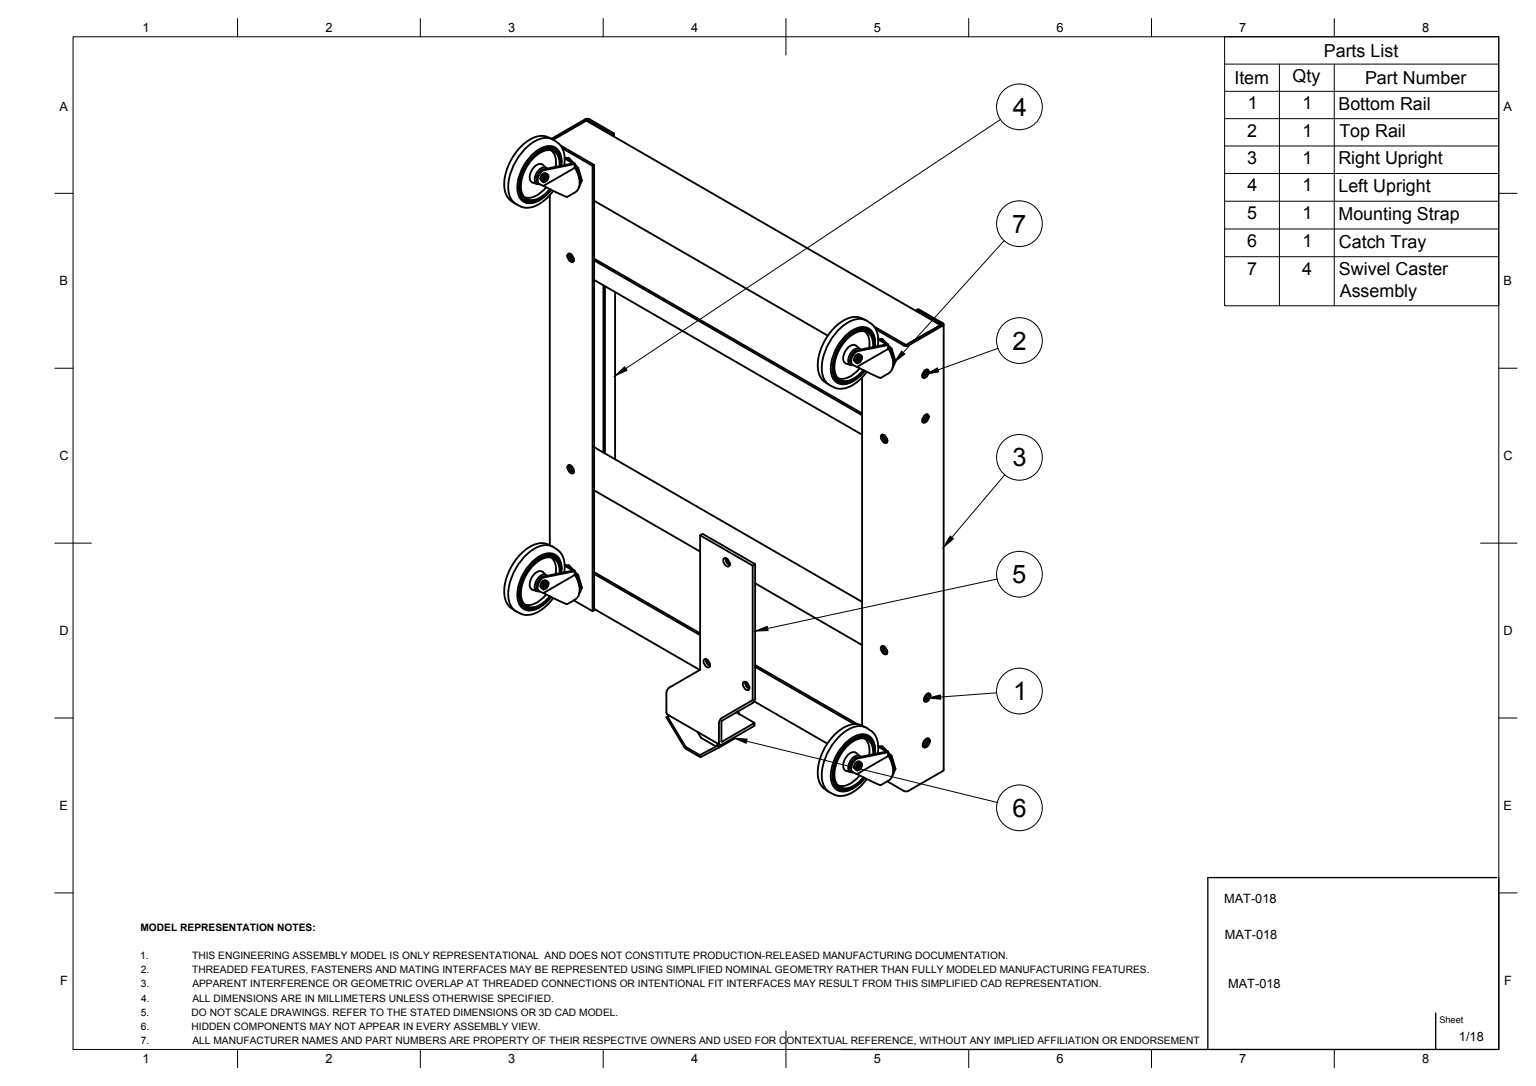
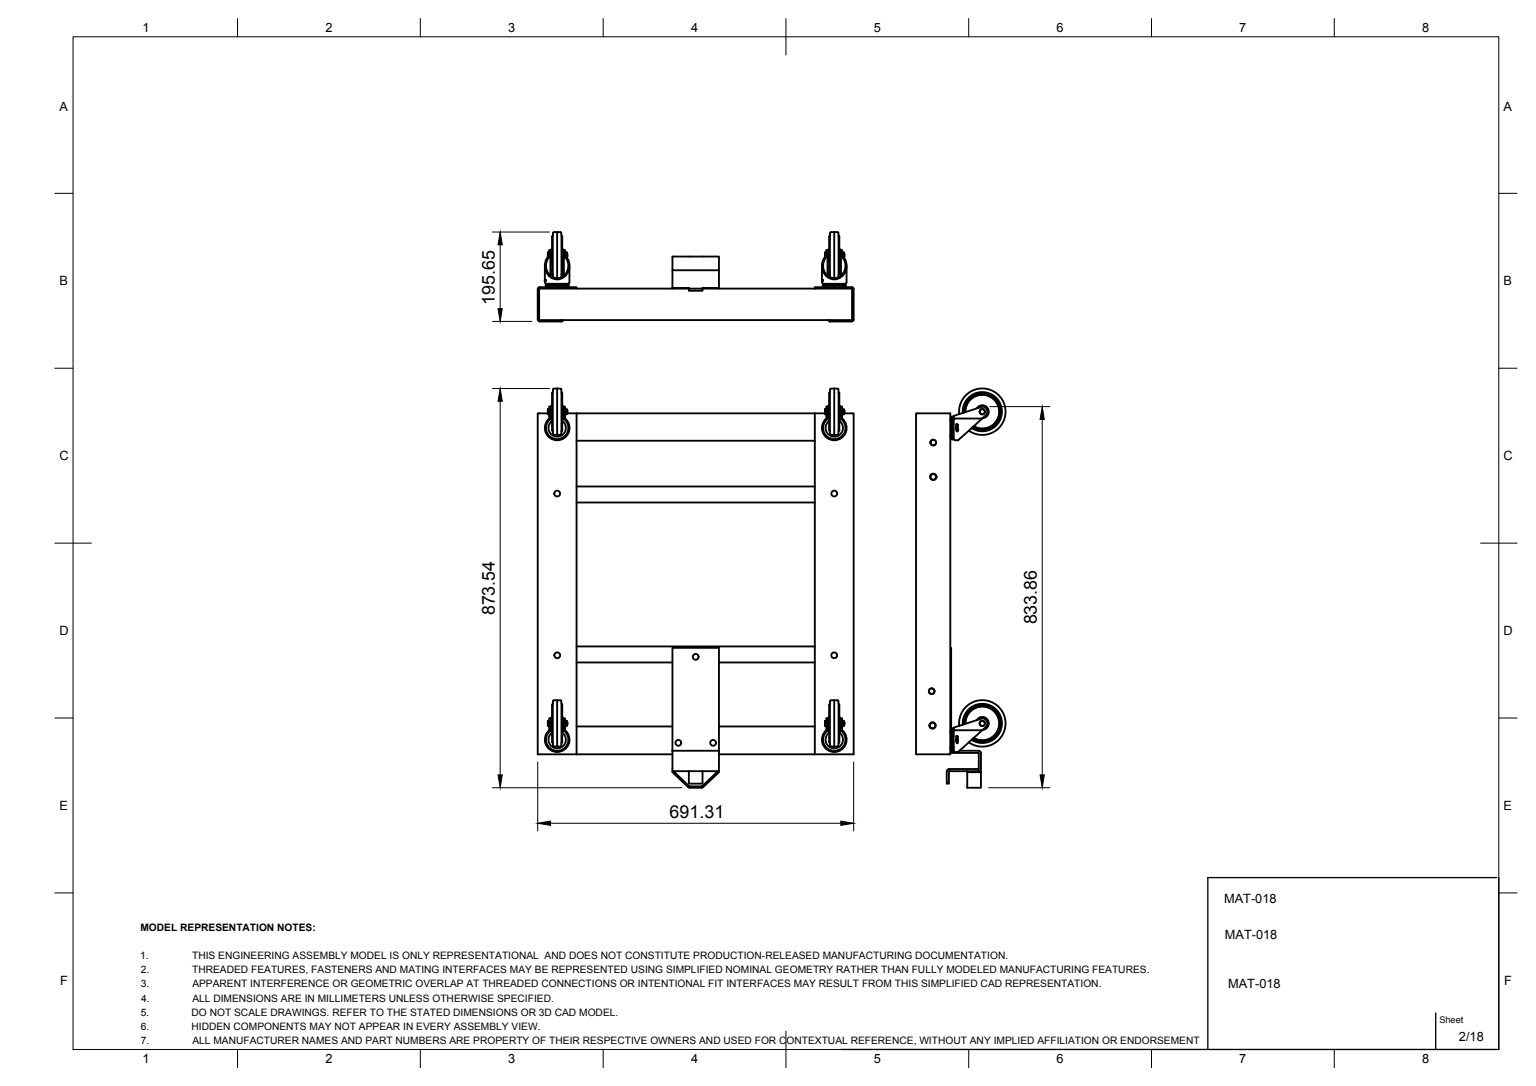
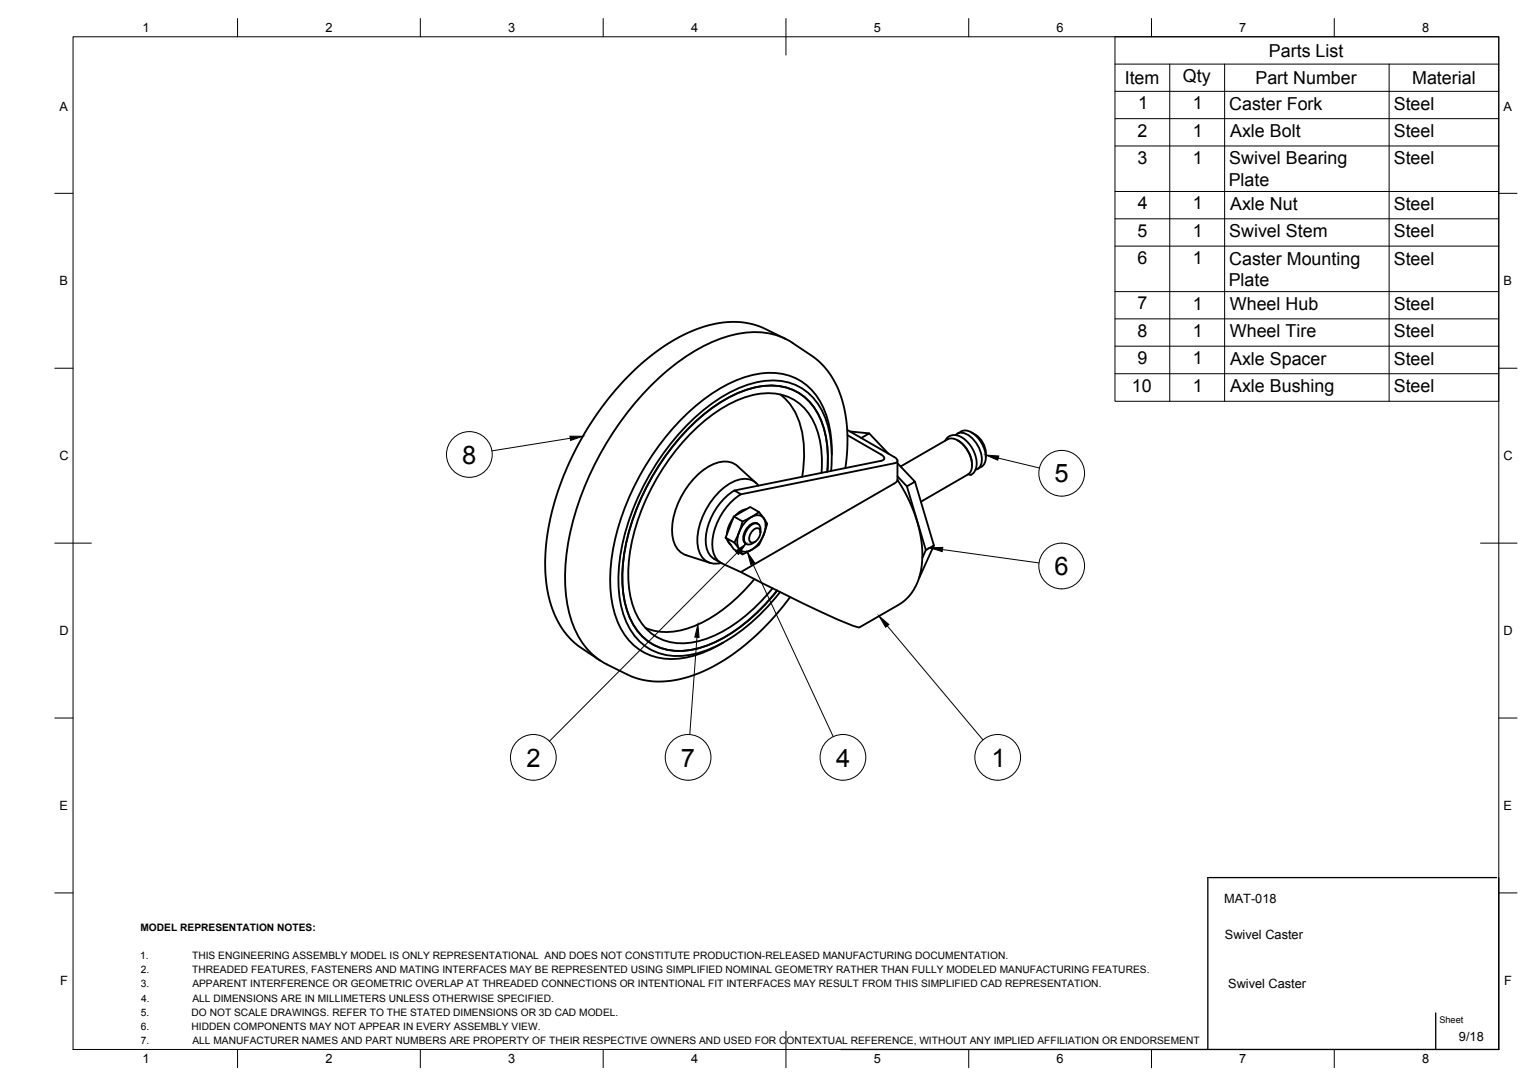
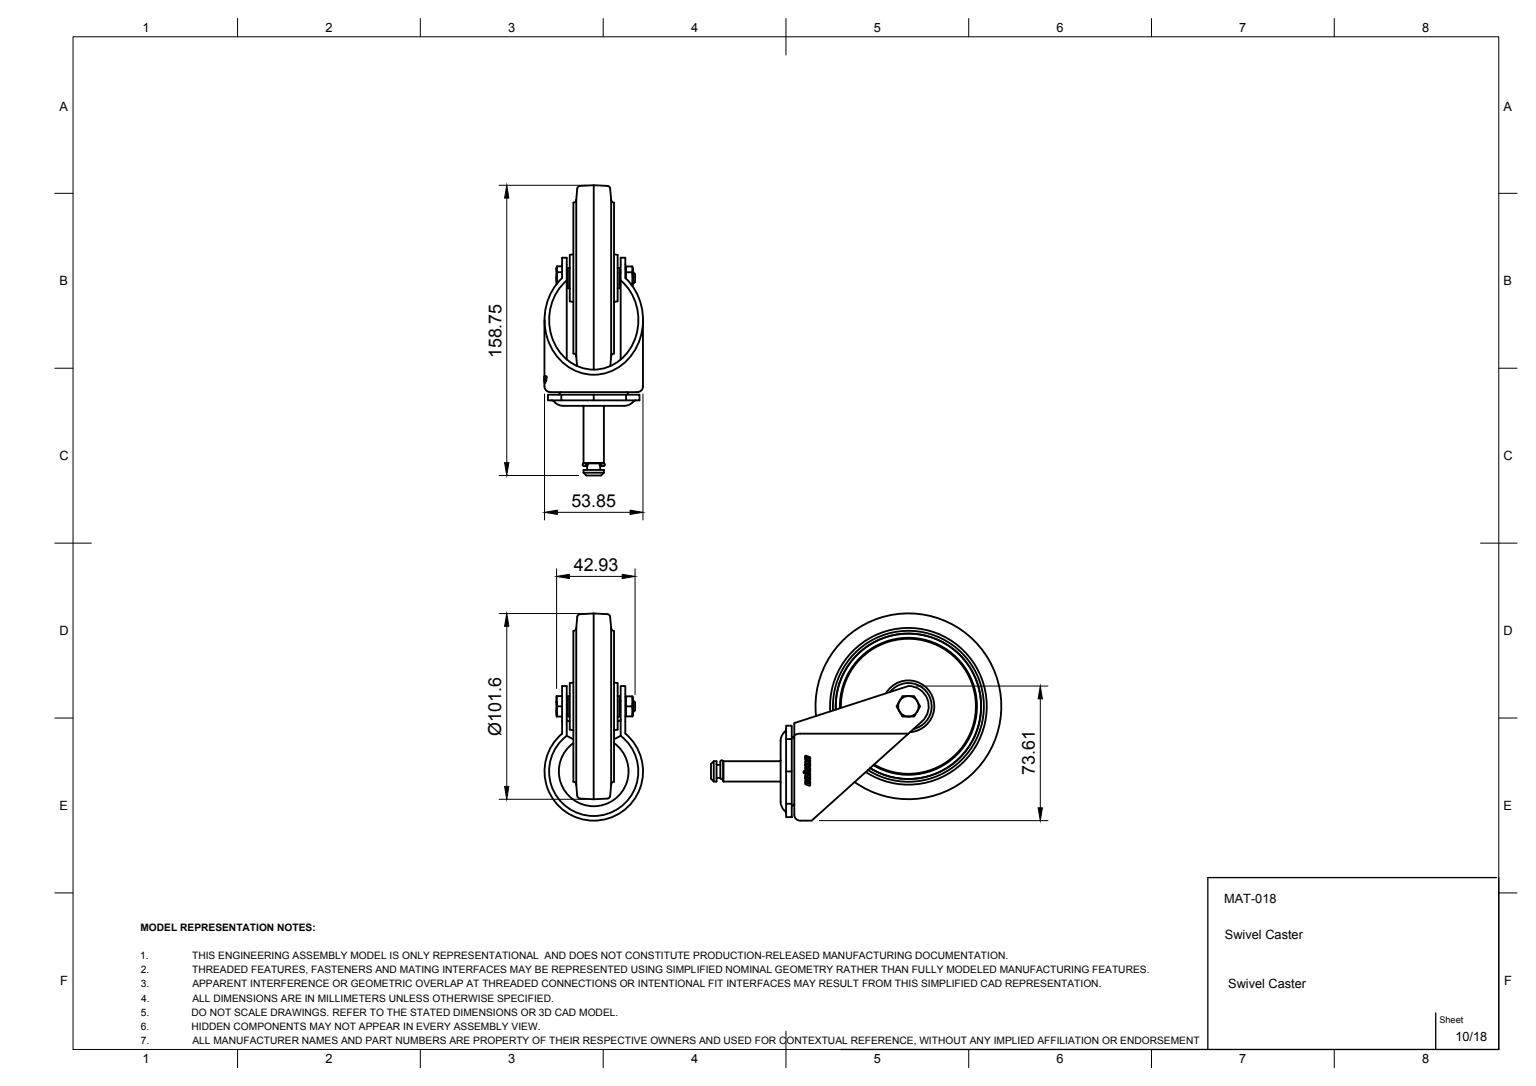
ISO-10303-21;
HEADER;
/* Generated by software containing ST-Developer
 * from STEP Tools, Inc. (www.steptools.com) 
 */

FILE_DESCRIPTION(
/* description */ ('STEP AP214'),
/* implementation_level */ '2;1');

FILE_NAME(
/* name */ 'MAT-018.step',
/* time_stamp */ '2026-11-14T06:16:09-08:00',
/* author */ (''),
/* organization */ (''),
/* preprocessor_version */ 'ST-DEVELOPER v20.2',
/* originating_system */ 'Autodesk Translation Framework v15.17.0.0',
/* authorisation */ '');

FILE_SCHEMA (('AUTOMOTIVE_DESIGN { 1 0 10303 214 3 1 1 }'));
ENDSEC;

DATA;
#10=MECHANICAL_DESIGN_GEOMETRIC_PRESENTATION_REPRESENTATION('',(#347,#348,
#349,#350,#351,#352,#353,#354,#355,#356,#357,#358,#359,#360,#361,#362),
#18006);
#11=ITEM_DEFINED_TRANSFORMATION($,$,#10244,#10840);
#12=ITEM_DEFINED_TRANSFORMATION($,$,#10508,#10841);
#13=ITEM_DEFINED_TRANSFORMATION($,$,#10546,#10842);
#14=ITEM_DEFINED_TRANSFORMATION($,$,#10592,#10843);
#15=ITEM_DEFINED_TRANSFORMATION($,$,#10635,#10844);
#16=ITEM_DEFINED_TRANSFORMATION($,$,#10683,#10845);
#17=ITEM_DEFINED_TRANSFORMATION($,$,#10733,#10846);
#18=ITEM_DEFINED_TRANSFORMATION($,$,#10772,#10847);
#19=ITEM_DEFINED_TRANSFORMATION($,$,#10817,#10848);
#20=ITEM_DEFINED_TRANSFORMATION($,$,#10826,#10849);
#21=ITEM_DEFINED_TRANSFORMATION($,$,#10243,#10850);
#22=ITEM_DEFINED_TRANSFORMATION($,$,#9750,#10851);
#23=ITEM_DEFINED_TRANSFORMATION($,$,#9886,#10852);
#24=ITEM_DEFINED_TRANSFORMATION($,$,#10013,#10853);
#25=ITEM_DEFINED_TRANSFORMATION($,$,#10080,#10854);
#26=ITEM_DEFINED_TRANSFORMATION($,$,#10147,#10855);
#27=ITEM_DEFINED_TRANSFORMATION($,$,#10211,#10856);
#28=ITEM_DEFINED_TRANSFORMATION($,$,#10242,#10857);
#29=ITEM_DEFINED_TRANSFORMATION($,$,#10242,#10858);
#30=ITEM_DEFINED_TRANSFORMATION($,$,#10242,#10859);
#31=ITEM_DEFINED_TRANSFORMATION($,$,#10242,#10860);
#32=(
REPRESENTATION_RELATIONSHIP($,$,#18079,#18078)
REPRESENTATION_RELATIONSHIP_WITH_TRANSFORMATION(#11)
SHAPE_REPRESENTATION_RELATIONSHIP()
);
#33=(
REPRESENTATION_RELATIONSHIP($,$,#18080,#18078)
REPRESENTATION_RELATIONSHIP_WITH_TRANSFORMATION(#12)
SHAPE_REPRESENTATION_RELATIONSHIP()
);
#34=(
REPRESENTATION_RELATIONSHIP($,$,#18081,#18078)
REPRESENTATION_RELATIONSHIP_WITH_TRANSFORMATION(#13)
SHAPE_REPRESENTATION_RELATIONSHIP()
);
#35=(
REPRESENTATION_RELATIONSHIP($,$,#18082,#18078)
REPRESENTATION_RELATIONSHIP_WITH_TRANSFORMATION(#14)
SHAPE_REPRESENTATION_RELATIONSHIP()
);
#36=(
REPRESENTATION_RELATIONSHIP($,$,#18083,#18078)
REPRESENTATION_RELATIONSHIP_WITH_TRANSFORMATION(#15)
SHAPE_REPRESENTATION_RELATIONSHIP()
);
#37=(
REPRESENTATION_RELATIONSHIP($,$,#18084,#18078)
REPRESENTATION_RELATIONSHIP_WITH_TRANSFORMATION(#16)
SHAPE_REPRESENTATION_RELATIONSHIP()
);
#38=(
REPRESENTATION_RELATIONSHIP($,$,#18085,#18078)
REPRESENTATION_RELATIONSHIP_WITH_TRANSFORMATION(#17)
SHAPE_REPRESENTATION_RELATIONSHIP()
);
#39=(
REPRESENTATION_RELATIONSHIP($,$,#18086,#18078)
REPRESENTATION_RELATIONSHIP_WITH_TRANSFORMATION(#18)
SHAPE_REPRESENTATION_RELATIONSHIP()
);
#40=(
REPRESENTATION_RELATIONSHIP($,$,#18087,#18078)
REPRESENTATION_RELATIONSHIP_WITH_TRANSFORMATION(#19)
SHAPE_REPRESENTATION_RELATIONSHIP()
);
#41=(
REPRESENTATION_RELATIONSHIP($,$,#18088,#18078)
REPRESENTATION_RELATIONSHIP_WITH_TRANSFORMATION(#20)
SHAPE_REPRESENTATION_RELATIONSHIP()
);
#42=(
REPRESENTATION_RELATIONSHIP($,$,#18078,#18077)
REPRESENTATION_RELATIONSHIP_WITH_TRANSFORMATION(#21)
SHAPE_REPRESENTATION_RELATIONSHIP()
);
#43=(
REPRESENTATION_RELATIONSHIP($,$,#18071,#18070)
REPRESENTATION_RELATIONSHIP_WITH_TRANSFORMATION(#22)
SHAPE_REPRESENTATION_RELATIONSHIP()
);
#44=(
REPRESENTATION_RELATIONSHIP($,$,#18072,#18070)
REPRESENTATION_RELATIONSHIP_WITH_TRANSFORMATION(#23)
SHAPE_REPRESENTATION_RELATIONSHIP()
);
#45=(
REPRESENTATION_RELATIONSHIP($,$,#18073,#18070)
REPRESENTATION_RELATIONSHIP_WITH_TRANSFORMATION(#24)
SHAPE_REPRESENTATION_RELATIONSHIP()
);
#46=(
REPRESENTATION_RELATIONSHIP($,$,#18074,#18070)
REPRESENTATION_RELATIONSHIP_WITH_TRANSFORMATION(#25)
SHAPE_REPRESENTATION_RELATIONSHIP()
);
#47=(
REPRESENTATION_RELATIONSHIP($,$,#18075,#18070)
REPRESENTATION_RELATIONSHIP_WITH_TRANSFORMATION(#26)
SHAPE_REPRESENTATION_RELATIONSHIP()
);
#48=(
REPRESENTATION_RELATIONSHIP($,$,#18076,#18070)
REPRESENTATION_RELATIONSHIP_WITH_TRANSFORMATION(#27)
SHAPE_REPRESENTATION_RELATIONSHIP()
);
#49=(
REPRESENTATION_RELATIONSHIP($,$,#18077,#18070)
REPRESENTATION_RELATIONSHIP_WITH_TRANSFORMATION(#28)
SHAPE_REPRESENTATION_RELATIONSHIP()
);
#50=(
REPRESENTATION_RELATIONSHIP($,$,#18077,#18070)
REPRESENTATION_RELATIONSHIP_WITH_TRANSFORMATION(#29)
SHAPE_REPRESENTATION_RELATIONSHIP()
);
#51=(
REPRESENTATION_RELATIONSHIP($,$,#18077,#18070)
REPRESENTATION_RELATIONSHIP_WITH_TRANSFORMATION(#30)
SHAPE_REPRESENTATION_RELATIONSHIP()
);
#52=(
REPRESENTATION_RELATIONSHIP($,$,#18077,#18070)
REPRESENTATION_RELATIONSHIP_WITH_TRANSFORMATION(#31)
SHAPE_REPRESENTATION_RELATIONSHIP()
);
#53=CONTEXT_DEPENDENT_SHAPE_REPRESENTATION(#32,#18049);
#54=CONTEXT_DEPENDENT_SHAPE_REPRESENTATION(#33,#18050);
#55=CONTEXT_DEPENDENT_SHAPE_REPRESENTATION(#34,#18051);
#56=CONTEXT_DEPENDENT_SHAPE_REPRESENTATION(#35,#18052);
#57=CONTEXT_DEPENDENT_SHAPE_REPRESENTATION(#36,#18053);
#58=CONTEXT_DEPENDENT_SHAPE_REPRESENTATION(#37,#18054);
#59=CONTEXT_DEPENDENT_SHAPE_REPRESENTATION(#38,#18055);
#60=CONTEXT_DEPENDENT_SHAPE_REPRESENTATION(#39,#18056);
#61=CONTEXT_DEPENDENT_SHAPE_REPRESENTATION(#40,#18057);
#62=CONTEXT_DEPENDENT_SHAPE_REPRESENTATION(#41,#18058);
#63=CONTEXT_DEPENDENT_SHAPE_REPRESENTATION(#42,#18059);
#64=CONTEXT_DEPENDENT_SHAPE_REPRESENTATION(#43,#18060);
#65=CONTEXT_DEPENDENT_SHAPE_REPRESENTATION(#44,#18061);
#66=CONTEXT_DEPENDENT_SHAPE_REPRESENTATION(#45,#18062);
#67=CONTEXT_DEPENDENT_SHAPE_REPRESENTATION(#46,#18063);
#68=CONTEXT_DEPENDENT_SHAPE_REPRESENTATION(#47,#18064);
#69=CONTEXT_DEPENDENT_SHAPE_REPRESENTATION(#48,#18065);
#70=CONTEXT_DEPENDENT_SHAPE_REPRESENTATION(#49,#18066);
#71=CONTEXT_DEPENDENT_SHAPE_REPRESENTATION(#50,#18067);
#72=CONTEXT_DEPENDENT_SHAPE_REPRESENTATION(#51,#18068);
#73=CONTEXT_DEPENDENT_SHAPE_REPRESENTATION(#52,#18069);
#74=NEXT_ASSEMBLY_USAGE_OCCURRENCE('Caster Fork:1','Caster Fork:1',
'Caster Fork:1',#18098,#18099,'Caster Fork:1');
#75=NEXT_ASSEMBLY_USAGE_OCCURRENCE('Axle Bolt:1','Axle Bolt:1',
'Axle Bolt:1',#18098,#18100,'Axle Bolt:1');
#76=NEXT_ASSEMBLY_USAGE_OCCURRENCE('Swivel Bearing Plate:1',
'Swivel Bearing Plate:1','Swivel Bearing Plate:1',#18098,#18101,
'Swivel Bearing Plate:1');
#77=NEXT_ASSEMBLY_USAGE_OCCURRENCE('Axle Nut:1','Axle Nut:1',
'Axle Nut:1',#18098,#18102,'Axle Nut:1');
#78=NEXT_ASSEMBLY_USAGE_OCCURRENCE('Swivel Stem:1','Swivel Stem:1',
'Swivel Stem:1',#18098,#18103,'Swivel Stem:1');
#79=NEXT_ASSEMBLY_USAGE_OCCURRENCE('Caster Mounting Plate:1',
'Caster Mounting Plate:1','Caster Mounting Plate:1',#18098,#18104,
'Caster Mounting Plate:1');
#80=NEXT_ASSEMBLY_USAGE_OCCURRENCE('Wheel Hub:1','Wheel Hub:1',
'Wheel Hub:1',#18098,#18105,'Wheel Hub:1');
#81=NEXT_ASSEMBLY_USAGE_OCCURRENCE('Wheel Tire:1','Wheel Tire:1',
'Wheel Tire:1',#18098,#18106,'Wheel Tire:1');
#82=NEXT_ASSEMBLY_USAGE_OCCURRENCE('Axle Spacer:1','Axle Spacer:1',
'Axle Spacer:1',#18098,#18107,'Axle Spacer:1');
#83=NEXT_ASSEMBLY_USAGE_OCCURRENCE('Axle Bushing:1','Axle Bushing:1',
'Axle Bushing:1',#18098,#18108,'Axle Bushing:1');
#84=NEXT_ASSEMBLY_USAGE_OCCURRENCE('Swivel Caster:1','Swivel Caster:1',
'Swivel Caster:1',#18097,#18098,'Swivel Caster:1');
#85=NEXT_ASSEMBLY_USAGE_OCCURRENCE('Bottom Rail:1','Bottom Rail:1',
'Bottom Rail:1',#18090,#18091,'Bottom Rail:1');
#86=NEXT_ASSEMBLY_USAGE_OCCURRENCE('Top Rail:1','Top Rail:1',
'Top Rail:1',#18090,#18092,'Top Rail:1');
#87=NEXT_ASSEMBLY_USAGE_OCCURRENCE('Right Upright:1','Right Upright:1',
'Right Upright:1',#18090,#18093,'Right Upright:1');
#88=NEXT_ASSEMBLY_USAGE_OCCURRENCE('Left Upright:1','Left Upright:1',
'Left Upright:1',#18090,#18094,'Left Upright:1');
#89=NEXT_ASSEMBLY_USAGE_OCCURRENCE('Mounting Strap:1',
'Mounting Strap:1','Mounting Strap:1',#18090,#18095,'Mounting Strap:1');
#90=NEXT_ASSEMBLY_USAGE_OCCURRENCE('Catch Tray:1','Catch Tray:1',
'Catch Tray:1',#18090,#18096,'Catch Tray:1');
#91=NEXT_ASSEMBLY_USAGE_OCCURRENCE('Swivel Caster Assembly:1',
'Swivel Caster Assembly:1','Swivel Caster Assembly:1',#18090,#18097,
'Swivel Caster Assembly:1');
#92=NEXT_ASSEMBLY_USAGE_OCCURRENCE('Swivel Caster Assembly:2',
'Swivel Caster Assembly:2','Swivel Caster Assembly:2',#18090,#18097,
'Swivel Caster Assembly:2');
#93=NEXT_ASSEMBLY_USAGE_OCCURRENCE('Swivel Caster Assembly:3',
'Swivel Caster Assembly:3','Swivel Caster Assembly:3',#18090,#18097,
'Swivel Caster Assembly:3');
#94=NEXT_ASSEMBLY_USAGE_OCCURRENCE('Swivel Caster Assembly:4',
'Swivel Caster Assembly:4','Swivel Caster Assembly:4',#18090,#18097,
'Swivel Caster Assembly:4');
#95=(
BOUNDED_CURVE()
B_SPLINE_CURVE(2,(#17284,#17285,#17286),.UNSPECIFIED.,.F.,.F.)
B_SPLINE_CURVE_WITH_KNOTS((3,3),(-2.0333659945968,-1.31472121783515),
 .UNSPECIFIED.)
CURVE()
GEOMETRIC_REPRESENTATION_ITEM()
RATIONAL_B_SPLINE_CURVE((2.35176643423756,2.35176643423756,2.18291720111281))
REPRESENTATION_ITEM('')
);
#96=(
BOUNDED_CURVE()
B_SPLINE_CURVE(2,(#17288,#17289,#17290),.UNSPECIFIED.,.F.,.F.)
B_SPLINE_CURVE_WITH_KNOTS((3,3),(-2.75201077135845,-2.0333659945968),
 .UNSPECIFIED.)
CURVE()
GEOMETRIC_REPRESENTATION_ITEM()
RATIONAL_B_SPLINE_CURVE((2.18291720111281,2.35176643423756,2.35176643423756))
REPRESENTATION_ITEM('')
);
#97=(
BOUNDED_CURVE()
B_SPLINE_CURVE(2,(#17304,#17305,#17306),.UNSPECIFIED.,.F.,.F.)
B_SPLINE_CURVE_WITH_KNOTS((3,3),(-2.0333659945968,-1.31472121783515),
 .UNSPECIFIED.)
CURVE()
GEOMETRIC_REPRESENTATION_ITEM()
RATIONAL_B_SPLINE_CURVE((2.35176643423756,2.35176643423756,2.18291720111281))
REPRESENTATION_ITEM('')
);
#98=(
BOUNDED_CURVE()
B_SPLINE_CURVE(2,(#17307,#17308,#17309),.UNSPECIFIED.,.F.,.F.)
B_SPLINE_CURVE_WITH_KNOTS((3,3),(-2.75201077135845,-2.0333659945968),
 .UNSPECIFIED.)
CURVE()
GEOMETRIC_REPRESENTATION_ITEM()
RATIONAL_B_SPLINE_CURVE((2.18291720111281,2.35176643423756,2.35176643423756))
REPRESENTATION_ITEM('')
);
#99=(
BOUNDED_CURVE()
B_SPLINE_CURVE(2,(#17312,#17313,#17314),.UNSPECIFIED.,.F.,.F.)
B_SPLINE_CURVE_WITH_KNOTS((3,3),(-2.0333659945968,-1.31472121783515),
 .UNSPECIFIED.)
CURVE()
GEOMETRIC_REPRESENTATION_ITEM()
RATIONAL_B_SPLINE_CURVE((2.35176643423756,2.35176643423756,2.18291720111281))
REPRESENTATION_ITEM('')
);
#100=(
BOUNDED_CURVE()
B_SPLINE_CURVE(2,(#17315,#17316,#17317),.UNSPECIFIED.,.F.,.F.)
B_SPLINE_CURVE_WITH_KNOTS((3,3),(-2.75201077135844,-2.03336599459679),
 .UNSPECIFIED.)
CURVE()
GEOMETRIC_REPRESENTATION_ITEM()
RATIONAL_B_SPLINE_CURVE((2.18291720111281,2.35176643423757,2.35176643423757))
REPRESENTATION_ITEM('')
);
#101=(
BOUNDED_CURVE()
B_SPLINE_CURVE(2,(#17320,#17321,#17322),.UNSPECIFIED.,.F.,.F.)
B_SPLINE_CURVE_WITH_KNOTS((3,3),(-2.03336599459679,-1.31472121783515),
 .UNSPECIFIED.)
CURVE()
GEOMETRIC_REPRESENTATION_ITEM()
RATIONAL_B_SPLINE_CURVE((2.35176643423756,2.35176643423756,2.18291720111281))
REPRESENTATION_ITEM('')
);
#102=(
BOUNDED_CURVE()
B_SPLINE_CURVE(2,(#17323,#17324,#17325),.UNSPECIFIED.,.F.,.F.)
B_SPLINE_CURVE_WITH_KNOTS((3,3),(-2.75201077135844,-2.0333659945968),
 .UNSPECIFIED.)
CURVE()
GEOMETRIC_REPRESENTATION_ITEM()
RATIONAL_B_SPLINE_CURVE((2.18291720111281,2.35176643423756,2.35176643423756))
REPRESENTATION_ITEM('')
);
#103=(
BOUNDED_CURVE()
B_SPLINE_CURVE(2,(#17328,#17329,#17330),.UNSPECIFIED.,.F.,.F.)
B_SPLINE_CURVE_WITH_KNOTS((3,3),(-2.0333659945968,-1.31472121783515),
 .UNSPECIFIED.)
CURVE()
GEOMETRIC_REPRESENTATION_ITEM()
RATIONAL_B_SPLINE_CURVE((2.35176643423756,2.35176643423756,2.18291720111281))
REPRESENTATION_ITEM('')
);
#104=(
BOUNDED_CURVE()
B_SPLINE_CURVE(2,(#17331,#17332,#17333),.UNSPECIFIED.,.F.,.F.)
B_SPLINE_CURVE_WITH_KNOTS((3,3),(-2.75201077135844,-2.03336599459679),
 .UNSPECIFIED.)
CURVE()
GEOMETRIC_REPRESENTATION_ITEM()
RATIONAL_B_SPLINE_CURVE((2.18291720111281,2.35176643423757,2.35176643423757))
REPRESENTATION_ITEM('')
);
#105=(
BOUNDED_CURVE()
B_SPLINE_CURVE(2,(#17336,#17337,#17338),.UNSPECIFIED.,.F.,.F.)
B_SPLINE_CURVE_WITH_KNOTS((3,3),(-2.03336599459679,-1.31472121783515),
 .UNSPECIFIED.)
CURVE()
GEOMETRIC_REPRESENTATION_ITEM()
RATIONAL_B_SPLINE_CURVE((2.35176643423756,2.35176643423756,2.18291720111281))
REPRESENTATION_ITEM('')
);
#106=(
BOUNDED_CURVE()
B_SPLINE_CURVE(2,(#17339,#17340,#17341),.UNSPECIFIED.,.F.,.F.)
B_SPLINE_CURVE_WITH_KNOTS((3,3),(-2.75201077135844,-2.0333659945968),
 .UNSPECIFIED.)
CURVE()
GEOMETRIC_REPRESENTATION_ITEM()
RATIONAL_B_SPLINE_CURVE((2.18291720111281,2.35176643423756,2.35176643423756))
REPRESENTATION_ITEM('')
);
#107=(
BOUNDED_CURVE()
B_SPLINE_CURVE(2,(#17477,#17478,#17479),.UNSPECIFIED.,.F.,.F.)
B_SPLINE_CURVE_WITH_KNOTS((3,3),(-2.24923400345372,-1.47749762858512),
 .UNSPECIFIED.)
CURVE()
GEOMETRIC_REPRESENTATION_ITEM()
RATIONAL_B_SPLINE_CURVE((2.5632386809031,2.5632386809031,2.37920642358137))
REPRESENTATION_ITEM('')
);
#108=(
BOUNDED_CURVE()
B_SPLINE_CURVE(2,(#17481,#17482,#17483),.UNSPECIFIED.,.F.,.F.)
B_SPLINE_CURVE_WITH_KNOTS((3,3),(-3.02097037832232,-2.24923400345372),
 .UNSPECIFIED.)
CURVE()
GEOMETRIC_REPRESENTATION_ITEM()
RATIONAL_B_SPLINE_CURVE((2.37920642358137,2.5632386809031,2.5632386809031))
REPRESENTATION_ITEM('')
);
#109=(
BOUNDED_CURVE()
B_SPLINE_CURVE(2,(#17497,#17498,#17499),.UNSPECIFIED.,.F.,.F.)
B_SPLINE_CURVE_WITH_KNOTS((3,3),(-2.24923400345372,-1.47749762858512),
 .UNSPECIFIED.)
CURVE()
GEOMETRIC_REPRESENTATION_ITEM()
RATIONAL_B_SPLINE_CURVE((2.5632386809031,2.5632386809031,2.37920642358137))
REPRESENTATION_ITEM('')
);
#110=(
BOUNDED_CURVE()
B_SPLINE_CURVE(2,(#17500,#17501,#17502),.UNSPECIFIED.,.F.,.F.)
B_SPLINE_CURVE_WITH_KNOTS((3,3),(-3.02097037832232,-2.24923400345372),
 .UNSPECIFIED.)
CURVE()
GEOMETRIC_REPRESENTATION_ITEM()
RATIONAL_B_SPLINE_CURVE((2.37920642358137,2.5632386809031,2.5632386809031))
REPRESENTATION_ITEM('')
);
#111=(
BOUNDED_CURVE()
B_SPLINE_CURVE(2,(#17505,#17506,#17507),.UNSPECIFIED.,.F.,.F.)
B_SPLINE_CURVE_WITH_KNOTS((3,3),(-2.24923400345372,-1.47749762858512),
 .UNSPECIFIED.)
CURVE()
GEOMETRIC_REPRESENTATION_ITEM()
RATIONAL_B_SPLINE_CURVE((2.5632386809031,2.5632386809031,2.37920642358137))
REPRESENTATION_ITEM('')
);
#112=(
BOUNDED_CURVE()
B_SPLINE_CURVE(2,(#17508,#17509,#17510),.UNSPECIFIED.,.F.,.F.)
B_SPLINE_CURVE_WITH_KNOTS((3,3),(-3.02097037832232,-2.24923400345372),
 .UNSPECIFIED.)
CURVE()
GEOMETRIC_REPRESENTATION_ITEM()
RATIONAL_B_SPLINE_CURVE((2.37920642358137,2.5632386809031,2.5632386809031))
REPRESENTATION_ITEM('')
);
#113=(
BOUNDED_CURVE()
B_SPLINE_CURVE(2,(#17513,#17514,#17515),.UNSPECIFIED.,.F.,.F.)
B_SPLINE_CURVE_WITH_KNOTS((3,3),(-2.24923400345372,-1.47749762858512),
 .UNSPECIFIED.)
CURVE()
GEOMETRIC_REPRESENTATION_ITEM()
RATIONAL_B_SPLINE_CURVE((2.5632386809031,2.5632386809031,2.37920642358137))
REPRESENTATION_ITEM('')
);
#114=(
BOUNDED_CURVE()
B_SPLINE_CURVE(2,(#17516,#17517,#17518),.UNSPECIFIED.,.F.,.F.)
B_SPLINE_CURVE_WITH_KNOTS((3,3),(-3.02097037832232,-2.24923400345372),
 .UNSPECIFIED.)
CURVE()
GEOMETRIC_REPRESENTATION_ITEM()
RATIONAL_B_SPLINE_CURVE((2.37920642358137,2.5632386809031,2.5632386809031))
REPRESENTATION_ITEM('')
);
#115=(
BOUNDED_CURVE()
B_SPLINE_CURVE(2,(#17521,#17522,#17523),.UNSPECIFIED.,.F.,.F.)
B_SPLINE_CURVE_WITH_KNOTS((3,3),(-2.24923400345372,-1.47749762858512),
 .UNSPECIFIED.)
CURVE()
GEOMETRIC_REPRESENTATION_ITEM()
RATIONAL_B_SPLINE_CURVE((2.5632386809031,2.5632386809031,2.37920642358137))
REPRESENTATION_ITEM('')
);
#116=(
BOUNDED_CURVE()
B_SPLINE_CURVE(2,(#17524,#17525,#17526),.UNSPECIFIED.,.F.,.F.)
B_SPLINE_CURVE_WITH_KNOTS((3,3),(-3.02097037832232,-2.24923400345372),
 .UNSPECIFIED.)
CURVE()
GEOMETRIC_REPRESENTATION_ITEM()
RATIONAL_B_SPLINE_CURVE((2.37920642358137,2.5632386809031,2.5632386809031))
REPRESENTATION_ITEM('')
);
#117=(
BOUNDED_CURVE()
B_SPLINE_CURVE(2,(#17529,#17530,#17531),.UNSPECIFIED.,.F.,.F.)
B_SPLINE_CURVE_WITH_KNOTS((3,3),(-2.24923400345372,-1.47749762858512),
 .UNSPECIFIED.)
CURVE()
GEOMETRIC_REPRESENTATION_ITEM()
RATIONAL_B_SPLINE_CURVE((2.5632386809031,2.5632386809031,2.37920642358137))
REPRESENTATION_ITEM('')
);
#118=(
BOUNDED_CURVE()
B_SPLINE_CURVE(2,(#17532,#17533,#17534),.UNSPECIFIED.,.F.,.F.)
B_SPLINE_CURVE_WITH_KNOTS((3,3),(-3.02097037832232,-2.24923400345372),
 .UNSPECIFIED.)
CURVE()
GEOMETRIC_REPRESENTATION_ITEM()
RATIONAL_B_SPLINE_CURVE((2.37920642358137,2.5632386809031,2.5632386809031))
REPRESENTATION_ITEM('')
);
#119=CONICAL_SURFACE('',#10522,3.175,0.785398163397445);
#120=CONICAL_SURFACE('',#10524,5.588,1.30899693899575);
#121=CONICAL_SURFACE('',#10532,5.588,1.30899693899575);
#122=CONICAL_SURFACE('',#10533,5.588,1.30899693899575);
#123=CONICAL_SURFACE('',#10534,5.588,1.30899693899575);
#124=CONICAL_SURFACE('',#10535,5.588,1.30899693899575);
#125=CONICAL_SURFACE('',#10536,5.588,1.30899693899575);
#126=CONICAL_SURFACE('',#10555,9.59611131114252,0.375229267578829);
#127=CONICAL_SURFACE('',#10558,15.3208607241417,0.87573749484567);
#128=CONICAL_SURFACE('',#10579,8.56864389726312,0.349065850398865);
#129=CONICAL_SURFACE('',#10601,3.175,0.785398163397448);
#130=CONICAL_SURFACE('',#10607,2.48793,0.785398163397449);
#131=CONICAL_SURFACE('',#10609,5.4991,1.30899693899575);
#132=CONICAL_SURFACE('',#10617,5.4991,1.30899693899575);
#133=CONICAL_SURFACE('',#10618,5.4991,1.30899693899575);
#134=CONICAL_SURFACE('',#10619,5.4991,1.30899693899575);
#135=CONICAL_SURFACE('',#10620,5.4991,1.30899693899575);
#136=CONICAL_SURFACE('',#10621,5.4991,1.30899693899575);
#137=CONICAL_SURFACE('',#10642,5.30225,0.78539816339744);
#138=CONICAL_SURFACE('',#10645,4.03225,0.785398163397449);
#139=CONICAL_SURFACE('',#10665,9.525,0.785398163397447);
#140=CONICAL_SURFACE('',#10673,5.4991,0.899938860194128);
#141=CONICAL_SURFACE('',#10700,9.49667180024818,0.710179331162308);
#142=CONICAL_SURFACE('',#10715,11.0475234888716,0.521857699344453);
#143=CONICAL_SURFACE('',#10734,12.7,0.174532925199433);
#144=CONICAL_SURFACE('',#10737,36.9094469866104,0.0872664625997163);
#145=CONICAL_SURFACE('',#10755,37.465,0.0872664625997151);
#146=CONICAL_SURFACE('',#10758,14.1695751798421,0.174532925199433);
#147=CONICAL_SURFACE('',#10793,42.8625,1.48352986419518);
#148=CONICAL_SURFACE('',#10800,50.4073015581831,0.0523598775598306);
#149=CONICAL_SURFACE('',#10803,50.8,0.0523598775598286);
#150=CONICAL_SURFACE('',#10808,48.9603369133721,1.48352986419518);
#151=CONICAL_SURFACE('',#10827,6.0325,0.785398163397448);
#152=CONICAL_SURFACE('',#10833,5.6515,0.785398163397444);
#153=B_SPLINE_CURVE_WITH_KNOTS('',3,(#15200,#15201,#15202,#15203,#15204,
#15205,#15206,#15207,#15208,#15209,#15210,#15211,#15212,#15213),
 .UNSPECIFIED.,.F.,.F.,(4,2,2,2,2,2,4),(-1.05798753271501,-1.05709265506731,
-0.973736745413946,-0.891472788851149,-0.76069525606768,-0.641953226883473,
-0.528546327542565),.UNSPECIFIED.);
#154=B_SPLINE_CURVE_WITH_KNOTS('',3,(#15216,#15217,#15218,#15219,#15220,
#15221,#15222,#15223,#15224,#15225,#15226,#15227,#15228,#15229),
 .UNSPECIFIED.,.F.,.F.,(4,2,2,2,2,2,4),(-0.528546328245586,-0.415139428749977,
-0.296397399403776,-0.165619866441898,-0.0833559097668774,0.,0.00089487764896709),
 .UNSPECIFIED.);
#155=B_SPLINE_CURVE_WITH_KNOTS('',3,(#15238,#15239,#15240,#15241,#15242,
#15243,#15244,#15245,#15246,#15247,#15248,#15249,#15250),.UNSPECIFIED.,
 .F.,.F.,(4,3,2,2,2,4),(0.21085041130991,0.223006755891215,0.236570067983272,
0.250133380075328,0.264473984692125,0.278814589308922),.UNSPECIFIED.);
#156=B_SPLINE_CURVE_WITH_KNOTS('',3,(#15258,#15259,#15260,#15261,#15262,
#15263,#15264,#15265,#15266,#15267,#15268,#15269,#15270),.UNSPECIFIED.,
 .F.,.F.,(4,3,2,2,2,4),(0.0967470588752525,0.102352134988349,0.108680144531714,
0.115008154075079,0.121479335049924,0.12795051602477),.UNSPECIFIED.);
#157=B_SPLINE_CURVE_WITH_KNOTS('',3,(#15274,#15275,#15276,#15277,#15278,
#15279,#15280,#15281,#15282,#15283),.UNSPECIFIED.,.F.,.F.,(4,2,2,2,4),(0.0255773754096234,
0.0320941778505459,0.0386109802914685,0.04487288801887,0.0455317964599114),
 .UNSPECIFIED.);
#158=B_SPLINE_CURVE_WITH_KNOTS('',3,(#15295,#15296,#15297,#15298,#15299,
#15300,#15301,#15302,#15303,#15304),.UNSPECIFIED.,.F.,.F.,(4,2,2,2,4),(0.0555518948425541,
0.0697143696037577,0.0838768443649614,0.0974406410837565,0.0988633457096359),
 .UNSPECIFIED.);
#159=B_SPLINE_CURVE_WITH_KNOTS('',3,(#15308,#15309,#15310,#15311,#15312,
#15313,#15314,#15315,#15316,#15317,#15318,#15319,#15320),.UNSPECIFIED.,
 .F.,.F.,(4,3,2,2,2,4),(0.207540054652461,0.219669399137817,0.233251193765718,
0.246832988393618,0.260726192595137,0.274619396796655),.UNSPECIFIED.);
#160=B_SPLINE_CURVE_WITH_KNOTS('',3,(#15324,#15325,#15326,#15327,#15328,
#15329,#15330,#15331,#15332,#15333),.UNSPECIFIED.,.F.,.F.,(4,2,2,2,4),(0.16428763170294,
0.178102070080099,0.191916508457259,0.205501679135769,0.206962232527076),
 .UNSPECIFIED.);
#161=B_SPLINE_CURVE_WITH_KNOTS('',3,(#15337,#15338,#15339,#15340,#15341,
#15342,#15343,#15344,#15345,#15346,#15347,#15348),.UNSPECIFIED.,.F.,.F.,
(4,2,2,2,2,4),(-0.163559583041953,-0.149911541347083,-0.136263499652212,
-0.122657118337829,-0.109050737023445,-0.0969365731486168),
 .UNSPECIFIED.);
#162=B_SPLINE_CURVE_WITH_KNOTS('',3,(#15352,#15353,#15354,#15355,#15356,
#15357,#15358,#15359,#15360,#15361),.UNSPECIFIED.,.F.,.F.,(4,2,2,2,4),(0.0546379220841073,
0.0683206657449699,0.0820034094058326,0.095618453418336,0.097115409960504),
 .UNSPECIFIED.);
#163=B_SPLINE_CURVE_WITH_KNOTS('',3,(#15373,#15374,#15375,#15376,#15377,
#15378,#15379,#15380,#15381,#15382,#15383,#15384,#15385),.UNSPECIFIED.,
 .F.,.F.,(4,3,2,2,2,4),(0.0960584215960821,0.101656947163514,0.107962882036145,
0.114268816908776,0.120666041708234,0.127063266507691),.UNSPECIFIED.);
#164=B_SPLINE_CURVE_WITH_KNOTS('',3,(#15389,#15390,#15391,#15392,#15393,
#15394,#15395,#15396,#15397,#15398),.UNSPECIFIED.,.F.,.F.,(4,2,2,2,4),(0.0254225160875339,
0.0318310599511386,0.0382396038147433,0.0445505068754669,0.0452587541305585),
 .UNSPECIFIED.);
#165=B_SPLINE_CURVE_WITH_KNOTS('',3,(#15402,#15403,#15404,#15405,#15406,
#15407,#15408,#15409,#15410,#15411,#15412,#15413),.UNSPECIFIED.,.F.,.F.,
(4,2,2,2,2,4),(0.0453757700957857,0.0509777554095704,0.0572424460326272,
0.0635071366556841,0.069991368974924,0.0764756012941639),.UNSPECIFIED.);
#166=B_SPLINE_CURVE_WITH_KNOTS('',3,(#15417,#15418,#15419,#15420,#15421,
#15422,#15423,#15424,#15425,#15426),.UNSPECIFIED.,.F.,.F.,(4,2,2,2,4),(0.07642158870704,
0.082888389632956,0.089355190558872,0.0956194636605514,0.0962835621215226),
 .UNSPECIFIED.);
#167=B_SPLINE_CURVE_WITH_KNOTS('',3,(#15434,#15435,#15436,#15437,#15438,
#15439,#15440,#15441,#15442,#15443),.UNSPECIFIED.,.F.,.F.,(4,2,2,2,4),(0.165105174386134,
0.179022673216447,0.192940172046759,0.206516122272691,0.207964455891319),
 .UNSPECIFIED.);
#168=B_SPLINE_CURVE_WITH_KNOTS('',3,(#15447,#15448,#15449,#15450,#15451,
#15452,#15453,#15454,#15455,#15456,#15457,#15458),.UNSPECIFIED.,.F.,.F.,
(4,2,2,2,2,4),(-0.166550736130104,-0.152498247892531,-0.138445759654958,
-0.124723066292625,-0.111000372930291,-0.0988521866158088),
 .UNSPECIFIED.);
#169=B_SPLINE_CURVE_WITH_KNOTS('',3,(#15462,#15463,#15464,#15465,#15466,
#15467,#15468,#15469,#15470,#15471),.UNSPECIFIED.,.F.,.F.,(4,2,2,2,4),(0.0552319193229079,
0.0693177010899006,0.0834034828568933,0.0969771504520487,0.0984099016110821),
 .UNSPECIFIED.);
#170=B_SPLINE_CURVE_WITH_KNOTS('',3,(#15475,#15476,#15477,#15478,#15479,
#15480,#15481,#15482,#15483,#15484,#15485,#15486,#15487),.UNSPECIFIED.,
 .F.,.F.,(4,3,2,2,2,4),(0.207322425307731,0.219445581566735,0.233084442830756,
0.246723304094777,0.260499776550424,0.274276249006071),.UNSPECIFIED.);
#171=B_SPLINE_CURVE_WITH_KNOTS('',3,(#15495,#15496,#15497,#15498,#15499,
#15500,#15501,#15502,#15503,#15504,#15505,#15506,#15507),.UNSPECIFIED.,
 .F.,.F.,(4,3,2,2,2,4),(0.205715370401278,0.217827820732331,0.231419194140737,
0.245010567549143,0.258641629025127,0.272272690501112),.UNSPECIFIED.);
#172=B_SPLINE_CURVE_WITH_KNOTS('',3,(#15511,#15512,#15513,#15514,#15515,
#15516,#15517,#15518,#15519,#15520),.UNSPECIFIED.,.F.,.F.,(4,2,2,2,4),(0.163596062711937,
0.177261642791301,0.190927222870665,0.204516589314865,0.205991763272733),
 .UNSPECIFIED.);
#173=B_SPLINE_CURVE_WITH_KNOTS('',3,(#15524,#15525,#15526,#15527,#15528,
#15529,#15530,#15531,#15532,#15533,#15534,#15535),.UNSPECIFIED.,.F.,.F.,
(4,2,2,2,2,4),(-0.164348295072572,-0.150588945321872,-0.136829595571171,
-0.123188335921558,-0.109547076271945,-0.0974223985777787),
 .UNSPECIFIED.);
#174=B_SPLINE_CURVE_WITH_KNOTS('',3,(#15539,#15540,#15541,#15542,#15543,
#15544,#15545,#15546,#15547,#15548),.UNSPECIFIED.,.F.,.F.,(4,2,2,2,4),(0.0546289177653794,
0.0683781304671273,0.0821273431688751,0.0957153140059365,0.0971825919874656),
 .UNSPECIFIED.);
#175=B_SPLINE_CURVE_WITH_KNOTS('',3,(#15552,#15553,#15554,#15555,#15556,
#15557,#15558,#15559,#15560,#15561,#15562,#15563),.UNSPECIFIED.,.F.,.F.,
(4,2,2,2,2,4),(-0.1581976552075,-0.14953859658713,-0.135944322867954,-0.122350438097707,
-0.108756553327459,-0.0966457183911671),.UNSPECIFIED.);
#176=B_SPLINE_CURVE_WITH_KNOTS('',3,(#15567,#15568,#15569,#15570,#15571,
#15572,#15573,#15574,#15575,#15576),.UNSPECIFIED.,.F.,.F.,(4,2,2,2,4),(0.0543867252046237,
0.067982476504709,0.0815782278047944,0.0951722925298618,0.0966554674666057),
 .UNSPECIFIED.);
#177=B_SPLINE_CURVE_WITH_KNOTS('',3,(#15580,#15581,#15582,#15583,#15584,
#15585,#15586,#15587,#15588,#15589,#15590,#15591,#15592),.UNSPECIFIED.,
 .F.,.F.,(4,3,2,2,2,4),(0.205804224466746,0.217919171018548,0.231526785869892,
0.245134400721236,0.258773542241859,0.272412683762482),.UNSPECIFIED.);
#178=B_SPLINE_CURVE_WITH_KNOTS('',3,(#15600,#15601,#15602,#15603,#15604,
#15605,#15606,#15607,#15608,#15609,#15610,#15611,#15612,#15613,#15614,#15615,
#15616,#15617,#15618,#15619,#15620,#15621,#15622,#15623,#15624,#15625,#15626,
#15627,#15628,#15629,#15630,#15631,#15632,#15633,#15634,#15635,#15636,#15637,
#15638,#15639,#15640,#15641,#15642,#15643,#15644,#15645,#15646,#15647,#15648),
 .UNSPECIFIED.,.F.,.F.,(4,3,3,3,3,3,3,3,3,3,3,3,3,3,3,3,4),(0.,2.61893547064141E-5,
5.23793413384783E-5,5.58383751490617E-5,8.20276764980591E-5,0.000108218767831614,
0.000111677234387562,0.000137892678614942,0.000164110772385426,0.000167513965690742,
0.000193773004384055,0.000220034861789034,0.000223410297983501,0.000251403971499176,
0.000279397645014851,0.00030439928997083,0.000318271065547474),
 .UNSPECIFIED.);
#179=B_SPLINE_CURVE_WITH_KNOTS('',3,(#15652,#15653,#15654,#15655,#15656,
#15657,#15658,#15659,#15660,#15661,#15662,#15663,#15664,#15665,#15666,#15667,
#15668,#15669,#15670,#15671,#15672,#15673,#15674,#15675,#15676,#15677,#15678,
#15679,#15680,#15681,#15682),.UNSPECIFIED.,.F.,.F.,(4,3,3,3,3,3,3,3,3,3,
4),(0.,2.62780568359485E-5,5.25567686851679E-5,5.60245769576452E-5,8.22826460935953E-5,
0.000108540974908011,0.00011205135344726,0.000140047997847787,0.000168044642248314,
0.000192332778060391,0.000202453063043279),.UNSPECIFIED.);
#180=B_SPLINE_CURVE_WITH_KNOTS('',3,(#15686,#15687,#15688,#15689,#15690,
#15691,#15692,#15693,#15694,#15695,#15696,#15697),.UNSPECIFIED.,.F.,.F.,
(4,2,2,2,2,4),(0.0446273761614327,0.0502172562500547,0.0564923474159883,
0.0627674385819219,0.0690459288966258,0.0730446845801043),.UNSPECIFIED.);
#181=B_SPLINE_CURVE_WITH_KNOTS('',3,(#15701,#15702,#15703,#15704,#15705,
#15706,#15707,#15708,#15709,#15710,#15711,#15712,#15713),.UNSPECIFIED.,
 .F.,.F.,(4,3,2,2,2,4),(0.205661183093538,0.217774871326039,0.231378172344526,
0.244981473363013,0.258605551105049,0.267282538931095),.UNSPECIFIED.);
#182=B_SPLINE_CURVE_WITH_KNOTS('',3,(#15717,#15718,#15719,#15720,#15721,
#15722,#15723,#15724,#15725,#15726),.UNSPECIFIED.,.F.,.F.,(4,2,2,2,4),(0.163262830275177,
0.176886285503613,0.190509740732049,0.204102940652365,0.205583159560348),
 .UNSPECIFIED.);
#183=B_SPLINE_CURVE_WITH_KNOTS('',3,(#15730,#15731,#15732,#15733,#15734,
#15735,#15736,#15737,#15738,#15739,#15740,#15741),.UNSPECIFIED.,.F.,.F.,
(4,2,2,2,2,4),(-0.163130149565264,-0.149535588647776,-0.135941027730287,
-0.122346971672616,-0.108752915614944,-0.0966419320482501),
 .UNSPECIFIED.);
#184=B_SPLINE_CURVE_WITH_KNOTS('',3,(#15749,#15750,#15751,#15752,#15753,
#15754,#15755,#15756,#15757,#15758,#15759,#15760),.UNSPECIFIED.,.F.,.F.,
(4,2,2,2,2,4),(0.0446139201958562,0.0502036335989734,0.0564775523632566,
0.0627514711275398,0.0690279742599127,0.0753044773922856),.UNSPECIFIED.);
#185=B_SPLINE_CURVE_WITH_KNOTS('',3,(#15764,#15765,#15766,#15767,#15768,
#15769,#15770,#15771,#15772,#15773,#15774,#15775,#15776,#15777,#15778,#15779,
#15780,#15781,#15782,#15783,#15784,#15785,#15786,#15787,#15788,#15789,#15790,
#15791,#15792,#15793,#15794),.UNSPECIFIED.,.F.,.F.,(4,3,3,3,3,3,3,3,3,3,
4),(2.27682456221956E-18,2.62611604330797E-5,5.25236119386904E-5,5.59919272014685E-5,
8.22484332471172E-5,0.000108505779042415,0.000111984406055697,0.000139975655185019,
0.00016796690431434,0.000192266307986708,0.000202413152921916),
 .UNSPECIFIED.);
#186=B_SPLINE_CURVE_WITH_KNOTS('',3,(#15798,#15799,#15800,#15801,#15802,
#15803,#15804,#15805,#15806,#15807,#15808,#15809,#15810,#15811,#15812,#15813,
#15814,#15815,#15816,#15817,#15818,#15819,#15820,#15821,#15822,#15823,#15824,
#15825,#15826,#15827,#15828,#15829,#15830,#15831,#15832,#15833,#15834,#15835,
#15836,#15837,#15838,#15839,#15840,#15841,#15842,#15843),.UNSPECIFIED.,
 .F.,.F.,(4,3,3,3,3,3,3,3,3,3,3,3,3,3,3,4),(0.,2.62056710562362E-5,5.24122459271672E-5,
5.58749072901349E-5,8.20805533656243E-5,0.000108287777349756,0.000111750103803527,
0.00013797157239734,0.000164195107714011,0.00016762405468435,0.00019387110049265,
0.000220120280732043,0.000223533576760988,0.000251514765402322,0.000279495954043657,
0.000295071232665503),.UNSPECIFIED.);
#187=B_SPLINE_CURVE_WITH_KNOTS('',3,(#15849,#15850,#15851,#15852,#15853,
#15854,#15855,#15856,#15857,#15858,#15859,#15860),.UNSPECIFIED.,.F.,.F.,
(4,2,2,2,2,4),(-0.163588460581617,-0.149918703223695,-0.136248945865774,
-0.122659843326177,-0.10907074078658,-0.0969553682010378),.UNSPECIFIED.);
#188=B_SPLINE_CURVE_WITH_KNOTS('',3,(#15865,#15866,#15867,#15868,#15869,
#15870,#15871,#15872,#15873,#15874,#15875,#15876),.UNSPECIFIED.,.F.,.F.,
(4,2,2,2,2,4),(0.02522364794674,0.0315600070621689,0.0378963661775978,0.0441670847637199,
0.0504378033498421,0.056031556378255),.UNSPECIFIED.);
#189=B_SPLINE_CURVE_WITH_KNOTS('',3,(#15880,#15881,#15882,#15883,#15884,
#15885,#15886,#15887,#15888,#15889,#15890,#15891),.UNSPECIFIED.,.F.,.F.,
(4,2,2,2,2,4),(-0.0560474223348667,-0.0504542824488712,-0.0441674824357687,
-0.0378806824226663,-0.0315564480902848,-0.0252322137579033),
 .UNSPECIFIED.);
#190=B_SPLINE_CURVE_WITH_KNOTS('',3,(#15897,#15898,#15899,#15900,#15901,
#15902,#15903,#15904,#15905,#15906,#15907,#15908),.UNSPECIFIED.,.F.,.F.,
(4,2,2,2,2,4),(0.0555264431134477,0.0697759764010379,0.084025509688628,
0.0975925952726502,0.111159680856672,0.123319838984262),.UNSPECIFIED.);
#191=B_SPLINE_CURVE_WITH_KNOTS('',3,(#15914,#15915,#15916,#15917,#15918,
#15919,#15920,#15921,#15922,#15923,#15924,#15925),.UNSPECIFIED.,.F.,.F.,
(4,2,2,2,2,4),(-0.0566352708009396,-0.051032411592176,-0.0447683390658066,
-0.0385042665394373,-0.0320054221406205,-0.0255065777418038),
 .UNSPECIFIED.);
#192=B_SPLINE_CURVE_WITH_KNOTS('',3,(#15930,#15931,#15932,#15933,#15934,
#15935,#15936,#15937,#15938,#15939,#15940,#15941),.UNSPECIFIED.,.F.,.F.,
(4,2,2,2,2,4),(0.0252072649814483,0.0315441698913498,0.0378810748012514,
0.0441524037465837,0.050423732691916,0.0560171029002878),.UNSPECIFIED.);
#193=B_SPLINE_CURVE_WITH_KNOTS('',3,(#15945,#15946,#15947,#15948,#15949,
#15950,#15951,#15952,#15953,#15954,#15955,#15956),.UNSPECIFIED.,.F.,.F.,
(4,2,2,2,2,4),(0.0448456008400242,0.0504392241694892,0.0567103715329265,
0.0629815188963638,0.0693226351640837,0.0756637514318036),.UNSPECIFIED.);
#194=B_SPLINE_CURVE_WITH_KNOTS('',3,(#15962,#15963,#15964,#15965,#15966,
#15967,#15968,#15969,#15970,#15971,#15972,#15973),.UNSPECIFIED.,.F.,.F.,
(4,2,2,2,2,4),(0.0547709631956495,0.0686014107648034,0.0824318583339573,
0.0960164164785591,0.109600974623161,0.121729895512297),.UNSPECIFIED.);
#195=B_SPLINE_CURVE_WITH_KNOTS('',3,(#15979,#15980,#15981,#15982,#15983,
#15984,#15985,#15986,#15987,#15988,#15989,#15990),.UNSPECIFIED.,.F.,.F.,
(4,2,2,2,2,4),(0.0543756988562886,0.0679703063435974,0.0815649138309062,
0.0951589831425968,0.108753052454287,0.120864046050129),.UNSPECIFIED.);
#196=B_SPLINE_CURVE_WITH_KNOTS('',3,(#15996,#15997,#15998,#15999,#16000,
#16001,#16002,#16003,#16004,#16005,#16006,#16007),.UNSPECIFIED.,.F.,.F.,
(4,2,2,2,2,4),(-0.0558087776823009,-0.0502188800483809,-0.0439437225233225,
-0.0376685649982641,-0.0313897836779405,-0.0273908754914149),
 .UNSPECIFIED.);
#197=B_SPLINE_CURVE_WITH_KNOTS('',3,(#16013,#16014,#16015,#16016,#16017,
#16018,#16019,#16020,#16021,#16022,#16023,#16024),.UNSPECIFIED.,.F.,.F.,
(4,2,2,2,2,4),(0.0593157911247595,0.0679748555424918,0.0815691568764464,
0.0951630435926456,0.108756930308845,0.120867766511413),.UNSPECIFIED.);
#198=B_SPLINE_CURVE_WITH_KNOTS('',3,(#16030,#16031,#16032,#16033,#16034,
#16035,#16036,#16037,#16038,#16039,#16040,#16041),.UNSPECIFIED.,.F.,.F.,
(4,2,2,2,2,4),(-0.0557941081156571,-0.0502043559092106,-0.0439304482554855,
-0.0376565406017603,-0.0313798779363301,-0.0251032152708999),
 .UNSPECIFIED.);
#199=B_SPLINE_CURVE_WITH_KNOTS('',3,(#16054,#16055,#16056,#16057,#16058,
#16059,#16060,#16061,#16062,#16063,#16064,#16065,#16066,#16067),
 .UNSPECIFIED.,.F.,.F.,(4,2,2,2,2,2,4),(-0.000907806723825812,0.,0.0861327565892462,
0.170934084426717,0.302285699149098,0.420326013215975,0.53254595873157),
 .UNSPECIFIED.);
#200=B_SPLINE_CURVE_WITH_KNOTS('',3,(#16070,#16071,#16072,#16073,#16074,
#16075,#16076,#16077,#16078,#16079,#16080,#16081,#16082,#16083),
 .UNSPECIFIED.,.F.,.F.,(4,2,2,2,2,2,4),(0.532545958333644,0.644765903763188,
0.762806217739553,0.894157832361222,0.978959160133672,1.0650919166569,1.06599972338003),
 .UNSPECIFIED.);
#201=B_SPLINE_CURVE_WITH_KNOTS('',3,(#16164,#16165,#16166,#16167,#16168,
#16169,#16170,#16171,#16172,#16173,#16174,#16175,#16176,#16177,#16178,#16179,
#16180,#16181,#16182,#16183,#16184,#16185,#16186,#16187,#16188,#16189,#16190,
#16191,#16192,#16193,#16194),.UNSPECIFIED.,.F.,.F.,(4,3,3,3,3,3,3,3,3,3,
4),(0.,2.62263408984961E-5,5.24546735552962E-5,5.59294154878842E-5,8.21749107319586E-5,
0.000108422373034421,0.000111856532863144,0.000139836798189191,0.000167817063515238,
0.000192176678723499,0.000202417981568665),.UNSPECIFIED.);
#202=B_SPLINE_CURVE_WITH_KNOTS('',3,(#16202,#16203,#16204,#16205,#16206,
#16207,#16208,#16209,#16210,#16211,#16212,#16213,#16214,#16215,#16216,#16217,
#16218,#16219,#16220,#16221,#16222,#16223,#16224,#16225,#16226,#16227,#16228,
#16229,#16230,#16231,#16232,#16233,#16234,#16235,#16236,#16237,#16238,#16239,
#16240,#16241,#16242,#16243,#16244,#16245,#16246,#16247),.UNSPECIFIED.,
 .F.,.F.,(4,3,3,3,3,3,3,3,3,3,3,3,3,3,3,4),(2.13563060504163E-18,2.62706118365419E-5,
5.25422317849148E-5,5.60055724034312E-5,8.22632468767231E-5,0.000108521420780006,
0.000112012653469487,0.000138244940280857,0.000164477575979964,0.000167995405480013,
0.000194203258604318,0.000220411823033185,0.000223923150888067,0.000251862794760903,
0.000279802438633739,0.000295079264564926),.UNSPECIFIED.);
#203=B_SPLINE_CURVE_WITH_KNOTS('',3,(#16256,#16257,#16258,#16259,#16260,
#16261,#16262,#16263,#16264,#16265),.UNSPECIFIED.,.F.,.F.,(4,2,2,2,4),(0.120878275316054,
0.122361460237932,0.135955538785907,0.149551415242624,0.16314729169934),
 .UNSPECIFIED.);
#204=B_SPLINE_CURVE_WITH_KNOTS('',3,(#16271,#16272,#16273,#16274,#16275,
#16276,#16277,#16278,#16279,#16280,#16281,#16282,#16283),.UNSPECIFIED.,
 .F.,.F.,(4,2,2,2,3,4),(0.16344554459355,0.177087696013552,0.190729847433554,
0.204338378989781,0.217946910546008,0.230062131569141),.UNSPECIFIED.);
#205=B_SPLINE_CURVE_WITH_KNOTS('',3,(#16288,#16289,#16290,#16291,#16292,
#16293,#16294,#16295,#16296,#16297,#16298,#16299,#16300,#16301,#16302,#16303,
#16304,#16305,#16306,#16307,#16308,#16309,#16310,#16311,#16312,#16313,#16314,
#16315,#16316,#16317,#16318,#16319,#16320,#16321,#16322,#16323,#16324,#16325,
#16326,#16327,#16328,#16329,#16330,#16331,#16332,#16333,#16334,#16335,#16336),
 .UNSPECIFIED.,.F.,.F.,(4,3,3,3,3,3,3,3,3,3,3,3,3,3,3,3,4),(0.,2.63066605675786E-5,
5.26144517821229E-5,5.60828380067807E-5,8.23744636863053E-5,0.000108666220788274,
0.000112167396800155,0.000138420369210082,0.000164672953555991,0.000168222587689466,
0.000194429431005337,0.000220636200006698,0.000224190783516547,0.000252127645728524,
0.0002800645079405,0.000304890396682416,0.000318280503391252),
 .UNSPECIFIED.);
#206=B_SPLINE_CURVE_WITH_KNOTS('',3,(#16352,#16353,#16354,#16355,#16356,
#16357,#16358,#16359,#16360,#16361,#16362,#16363,#16364,#16365,#16366,#16367,
#16368,#16369,#16370,#16371,#16372,#16373,#16374,#16375,#16376,#16377,#16378,
#16379,#16380,#16381,#16382),.UNSPECIFIED.,.F.,.F.,(4,3,3,3,3,3,3,3,3,3,
4),(0.,2.62199367278079E-5,5.2442017850133E-5,5.59226387686515E-5,8.21617436204465E-5,
0.000108403259060271,0.000111842843273962,0.000139821267047986,0.00016779969082201,
0.000192187361442712,0.00020245986591176),.UNSPECIFIED.);
#207=B_SPLINE_CURVE_WITH_KNOTS('',3,(#16393,#16394,#16395,#16396,#16397,
#16398,#16399,#16400,#16401,#16402,#16403,#16404,#16405),.UNSPECIFIED.,
 .F.,.F.,(4,2,2,2,3,4),(0.168281017205692,0.176970274988815,0.190607585903283,
0.204200283505296,0.217792981107309,0.229907470869343),.UNSPECIFIED.);
#208=B_SPLINE_CURVE_WITH_KNOTS('',3,(#16411,#16412,#16413,#16414,#16415,
#16416,#16417,#16418,#16419,#16420),.UNSPECIFIED.,.F.,.F.,(4,2,2,2,4),(0.0121131236464053,
0.0135931571065978,0.0271863142132075,0.0408117295708293,0.0544371449284511),
 .UNSPECIFIED.);
#209=B_SPLINE_CURVE_WITH_KNOTS('',3,(#16449,#16450,#16451,#16452,#16453,
#16454,#16455,#16456,#16457,#16458),.UNSPECIFIED.,.F.,.F.,(4,2,2,2,4),(0.121464063304098,
0.12297011726776,0.136599840855674,0.150317377138189,0.164034913420704),
 .UNSPECIFIED.);
#210=B_SPLINE_CURVE_WITH_KNOTS('',3,(#16464,#16465,#16466,#16467,#16468,
#16469,#16470,#16471,#16472,#16473,#16474,#16475,#16476),.UNSPECIFIED.,
 .F.,.F.,(4,2,2,2,3,4),(0.163399990036943,0.177024219712394,0.190648449387846,
0.204248956979152,0.217849464570459,0.229962022162275),.UNSPECIFIED.);
#211=B_SPLINE_CURVE_WITH_KNOTS('',3,(#16482,#16483,#16484,#16485,#16486,
#16487,#16488,#16489,#16490,#16491),.UNSPECIFIED.,.F.,.F.,(4,2,2,2,4),(0.0121144161976424,
0.0135890687064821,0.0271781374129765,0.0408484901993985,0.0545188429858204),
 .UNSPECIFIED.);
#212=B_SPLINE_CURVE_WITH_KNOTS('',3,(#16506,#16507,#16508,#16509,#16510,
#16511,#16512,#16513,#16514,#16515,#16516,#16517,#16518,#16519,#16520,#16521,
#16522,#16523,#16524,#16525,#16526,#16527,#16528,#16529,#16530,#16531,#16532,
#16533,#16534,#16535,#16536),.UNSPECIFIED.,.F.,.F.,(4,3,3,3,3,3,3,3,3,3,
4),(2.90921971083665E-18,2.61934841647759E-5,5.2395152029381E-5,5.59393582568155E-5,
8.23082290539125E-5,0.000108685833894815,0.000111857436416825,0.000139973890768046,
0.000168090345119268,0.00019281902375984,0.000203295197183654),
 .UNSPECIFIED.);
#213=B_SPLINE_CURVE_WITH_KNOTS('',3,(#16540,#16541,#16542,#16543,#16544,
#16545,#16546,#16547,#16548,#16549,#16550,#16551,#16552,#16553,#16554,#16555,
#16556,#16557,#16558,#16559,#16560,#16561,#16562,#16563,#16564,#16565,#16566,
#16567,#16568,#16569,#16570,#16571,#16572,#16573,#16574,#16575,#16576,#16577,
#16578,#16579,#16580,#16581,#16582,#16583,#16584,#16585,#16586,#16587,#16588),
 .UNSPECIFIED.,.F.,.F.,(4,3,3,3,3,3,3,3,3,3,3,3,3,3,3,3,4),(1.30104260698261E-18,
2.65431015818806E-5,5.30846524833209E-5,5.65518115748557E-5,8.29883809227767E-5,
0.000109420389342837,0.000113115409927836,0.000139395878445335,0.000165671077299507,
0.000169493795555906,0.000195635173123321,0.000221773198529148,0.000225528117581789,
0.000253396458511377,0.000281264799440966,0.000305945864598804,0.00031889992532713),
 .UNSPECIFIED.);
#214=B_SPLINE_CURVE_WITH_KNOTS('',3,(#16591,#16592,#16593,#16594,#16595,
#16596,#16597,#16598,#16599,#16600,#16601,#16602,#16603,#16604,#16605,#16606,
#16607,#16608,#16609,#16610,#16611,#16612,#16613,#16614,#16615,#16616,#16617,
#16618,#16619,#16620,#16621),.UNSPECIFIED.,.F.,.F.,(4,3,3,3,3,3,3,3,3,3,
4),(0.,2.6174265626545E-5,5.23571842467819E-5,5.59188941314991E-5,8.22683950090346E-5,
0.000108627984711294,0.000111816111086179,0.000139926889687584,0.00016803766828899,
0.000192852623046708,0.000203423599614867),.UNSPECIFIED.);
#215=B_SPLINE_CURVE_WITH_KNOTS('',3,(#16632,#16633,#16634,#16635,#16636,
#16637,#16638,#16639,#16640,#16641,#16642,#16643,#16644,#16645,#16646,#16647,
#16648,#16649,#16650,#16651,#16652,#16653,#16654,#16655,#16656,#16657,#16658,
#16659,#16660,#16661,#16662),.UNSPECIFIED.,.F.,.F.,(4,3,3,3,3,3,3,3,3,3,
4),(1.30104260698261E-18,2.65789018742066E-5,5.31575496968928E-5,5.66254500585291E-5,
8.3117956283313E-5,0.000109606128421635,0.000113260605340939,0.000141498061160802,
0.000169735516980665,0.000193794869906936,0.0002032455266205),
 .UNSPECIFIED.);
#216=B_SPLINE_CURVE_WITH_KNOTS('',3,(#16670,#16671,#16672,#16673,#16674,
#16675,#16676,#16677,#16678,#16679,#16680,#16681,#16682,#16683,#16684,#16685,
#16686,#16687,#16688,#16689,#16690,#16691,#16692,#16693,#16694,#16695,#16696,
#16697,#16698,#16699,#16700,#16701,#16702,#16703,#16704,#16705,#16706,#16707,
#16708,#16709,#16710,#16711,#16712,#16713,#16714,#16715,#16716,#16717,#16718),
 .UNSPECIFIED.,.F.,.F.,(4,3,3,3,3,3,3,3,3,3,3,3,3,3,3,3,4),(7.05981306231723E-18,
2.61006467232877E-5,5.22004452427167E-5,5.56427761810506E-5,8.17431350687009E-5,
0.000107846424934024,0.00011128691941793,0.000137455188613542,0.000163629521420686,
0.000166924412888132,0.000193226468602,0.000219536054997011,0.000222731064487749,
0.00025078237981636,0.000278833695144971,0.000304175189571627,0.000318860611922234),
 .UNSPECIFIED.);
#217=B_SPLINE_CURVE_WITH_KNOTS('',3,(#16725,#16726,#16727,#16728,#16729,
#16730,#16731,#16732,#16733,#16734,#16735,#16736,#16737,#16738,#16739,#16740,
#16741,#16742,#16743,#16744,#16745,#16746,#16747,#16748,#16749,#16750,#16751,
#16752,#16753,#16754,#16755,#16756,#16757,#16758),.UNSPECIFIED.,.F.,.F.,
(4,3,3,3,3,3,3,3,3,3,3,4),(0.,2.66309786063701E-5,5.32597578303729E-5,5.67266914086089E-5,
8.32237987914592E-5,0.000109714794420116,0.000113468211529127,0.00014030143344684,
0.000167116381203059,0.000169975455109431,0.000193999294088889,0.000203367690764691),
 .UNSPECIFIED.);
#218=B_SPLINE_CURVE_WITH_KNOTS('',3,(#16765,#16766,#16767,#16768,#16769,
#16770,#16771,#16772,#16773,#16774),.UNSPECIFIED.,.F.,.F.,(4,2,2,2,4),(0.122826993771593,
0.124381415276847,0.138086292496281,0.152074110944094,0.166061929391907),
 .UNSPECIFIED.);
#219=B_SPLINE_CURVE_WITH_KNOTS('',3,(#16780,#16781,#16782,#16783,#16784,
#16785,#16786,#16787,#16788,#16789,#16790,#16791,#16792),.UNSPECIFIED.,
 .F.,.F.,(4,2,2,2,3,4),(0.164716318384793,0.178505190418151,0.192294062451508,
0.205935985757488,0.219577909063469,0.231701904790623),.UNSPECIFIED.);
#220=B_SPLINE_CURVE_WITH_KNOTS('',3,(#16797,#16798,#16799,#16800,#16801,
#16802,#16803,#16804,#16805,#16806,#16807,#16808,#16809),.UNSPECIFIED.,
 .F.,.F.,(4,2,2,2,3,4),(0.0763169364557381,0.0827226314565487,0.0891283264573594,
0.0954364634280723,0.101744600398785,0.107343743760696),.UNSPECIFIED.);
#221=B_SPLINE_CURVE_WITH_KNOTS('',3,(#16825,#16826,#16827,#16828,#16829,
#16830,#16831,#16832,#16833,#16834),.UNSPECIFIED.,.F.,.F.,(4,2,2,2,4),(0.0565083181592569,
0.0571729351695743,0.0634384626468256,0.0699041737417157,0.0763698848366059),
 .UNSPECIFIED.);
#222=B_SPLINE_CURVE_WITH_KNOTS('',3,(#16844,#16845,#16846,#16847,#16848,
#16849,#16850,#16851,#16852,#16853),.UNSPECIFIED.,.F.,.F.,(4,2,2,2,4),(0.00560091332226562,
0.00626361772267091,0.0125272354453687,0.0190073781328202,0.0254875208202717),
 .UNSPECIFIED.);
#223=B_SPLINE_CURVE_WITH_KNOTS('',3,(#16862,#16863,#16864,#16865,#16866,
#16867,#16868,#16869,#16870,#16871),.UNSPECIFIED.,.F.,.F.,(4,2,2,2,4),(0.0121287728581793,
0.0135747504069423,0.027149500813912,0.0410891677145563,0.0550288346152006),
 .UNSPECIFIED.);
#224=B_SPLINE_CURVE_WITH_KNOTS('',3,(#16894,#16895,#16896,#16897,#16898,
#16899,#16900,#16901,#16902,#16903),.UNSPECIFIED.,.F.,.F.,(4,2,2,2,4),(0.123308394329165,
0.124726915019759,0.138288683222937,0.152491200248366,0.166693717273795),
 .UNSPECIFIED.);
#225=B_SPLINE_CURVE_WITH_KNOTS('',3,(#16909,#16910,#16911,#16912,#16913,
#16914,#16915,#16916,#16917,#16918,#16919,#16920,#16921),.UNSPECIFIED.,
 .F.,.F.,(4,2,2,2,3,4),(0.1674921196294,0.181685815580684,0.195879511531969,
0.209641890261917,0.223404268991865,0.235563977874896),.UNSPECIFIED.);
#226=B_SPLINE_CURVE_WITH_KNOTS('',3,(#16926,#16927,#16928,#16929,#16930,
#16931,#16932,#16933,#16934,#16935,#16936,#16937,#16938),.UNSPECIFIED.,
 .F.,.F.,(4,2,2,2,3,4),(0.0768568414287796,0.0834120101652974,0.0899671789018152,
0.096228821629629,0.102490464357443,0.108096650773217),.UNSPECIFIED.);
#227=B_SPLINE_CURVE_WITH_KNOTS('',3,(#16954,#16955,#16956,#16957,#16958,
#16959,#16960,#16961,#16962,#16963),.UNSPECIFIED.,.F.,.F.,(4,2,2,2,4),(0.0568054393240072,
0.0574625824337707,0.0637236753565987,0.070257488186888,0.0767913010171772),
 .UNSPECIFIED.);
#228=B_SPLINE_CURVE_WITH_KNOTS('',3,(#17013,#17014,#17015,#17016,#17017,
#17018,#17019,#17020,#17021,#17022,#17023,#17024,#17025,#17026,#17027,#17028,
#17029,#17030,#17031,#17032,#17033,#17034,#17035,#17036,#17037,#17038,#17039,
#17040,#17041,#17042,#17043),.UNSPECIFIED.,.F.,.F.,(4,3,3,3,3,3,3,3,3,3,
4),(0.,2.61513239163364E-5,5.23149693449337E-5,5.59191991956224E-5,8.23336238405149E-5,
0.000108762377139427,0.000111805968939859,0.000139992308701124,0.00016817864846239,
0.000193231131825241,0.000203961295469882),.UNSPECIFIED.);
#229=B_SPLINE_CURVE_WITH_KNOTS('',3,(#17045,#17046,#17047,#17048,#17049,
#17050,#17051,#17052,#17053,#17054,#17055,#17056,#17057,#17058,#17059,#17060,
#17061,#17062,#17063,#17064,#17065,#17066,#17067,#17068,#17069,#17070,#17071,
#17072,#17073,#17074,#17075,#17076,#17077,#17078),.UNSPECIFIED.,.F.,.F.,
(4,3,3,3,3,3,3,3,3,3,3,4),(0.,2.68288699039451E-5,5.36540568362787E-5,5.71203294509813E-5,
8.37529095566486E-5,0.000110375876221954,0.000114262444096402,0.000141133710037584,
0.000167982501687035,0.000171057322061712,0.000194929023159508,0.00020387754846829),
 .UNSPECIFIED.);
#230=B_SPLINE_CURVE_WITH_KNOTS('',3,(#17088,#17089,#17090,#17091,#17092,
#17093,#17094,#17095,#17096,#17097,#17098,#17099,#17100),.UNSPECIFIED.,
 .F.,.F.,(4,2,2,2,3,4),(0.0758223611140042,0.0821692755732936,0.0885161900325831,
0.0948103498137587,0.101104509594934,0.106699894517977),.UNSPECIFIED.);
#231=B_SPLINE_CURVE_WITH_KNOTS('',3,(#17102,#17103,#17104,#17105,#17106,
#17107,#17108,#17109,#17110,#17111,#17112,#17113,#17114),.UNSPECIFIED.,
 .F.,.F.,(4,3,2,2,2,4),(-0.00559501743802755,-2.0121057597855E-14,0.00629288428244951,
0.0125857685649191,0.0189280757524976,0.0252703829400761),.UNSPECIFIED.);
#232=B_SPLINE_CURVE_WITH_KNOTS('',3,(#17124,#17125,#17126,#17127,#17128,
#17129,#17130,#17131,#17132,#17133,#17134,#17135,#17136,#17137,#17138,#17139,
#17140,#17141,#17142,#17143,#17144,#17145,#17146,#17147,#17148,#17149,#17150,
#17151,#17152,#17153,#17154),.UNSPECIFIED.,.F.,.F.,(4,3,3,3,3,3,3,3,3,3,
4),(0.,2.61748461428238E-5,5.23614311506995E-5,5.5944332128628E-5,8.23825970679176E-5,
0.000108833515652107,0.000111856713001275,0.000140050102305964,0.000168243491610652,
0.000193188896321108,0.000203802255878226),.UNSPECIFIED.);
#233=B_SPLINE_CURVE_WITH_KNOTS('',3,(#17156,#17157,#17158,#17159,#17160,
#17161,#17162,#17163,#17164,#17165,#17166,#17167,#17168,#17169,#17170,#17171,
#17172,#17173,#17174,#17175,#17176,#17177,#17178,#17179,#17180,#17181,#17182,
#17183,#17184,#17185,#17186,#17187,#17188,#17189),.UNSPECIFIED.,.F.,.F.,
(4,3,3,3,3,3,3,3,3,3,3,4),(1.30104260698261E-18,2.67641714676527E-5,5.35270675426613E-5,
5.69941301136891E-5,8.36211550806795E-5,0.000110240768611593,0.000114003646822786,
0.000140905222888793,0.000167785530905218,0.000170759017810265,0.000194675460825806,
0.000203726362707034),.UNSPECIFIED.);
#234=B_SPLINE_CURVE_WITH_KNOTS('',3,(#17201,#17202,#17203,#17204,#17205,
#17206,#17207,#17208,#17209,#17210),.UNSPECIFIED.,.F.,.F.,(4,2,2,2,4),(-0.207068588326242,
-0.205609544125706,-0.19202493997465,-0.178195567968825,-0.164366195963),
 .UNSPECIFIED.);
#235=B_SPLINE_CURVE_WITH_KNOTS('',3,(#17214,#17215,#17216,#17217,#17218,
#17219,#17220,#17221,#17222,#17223,#17224,#17225,#17226),.UNSPECIFIED.,
 .F.,.F.,(4,2,2,2,3,4),(-0.0549894817446407,-0.0411565616169558,-0.027323641489271,
-0.0136618207446443,-1.75554015768853E-14,0.0121306256116926),
 .UNSPECIFIED.);
#236=B_SPLINE_CURVE_WITH_KNOTS('',3,(#17229,#17230,#17231,#17232,#17233,
#17234,#17235,#17236,#17237,#17238),.UNSPECIFIED.,.F.,.F.,(4,2,2,2,4),(-0.0971472763104068,
-0.0956493874579362,-0.0820329248805527,-0.068344233088617,-0.0546555412966814),
 .UNSPECIFIED.);
#237=TOROIDAL_SURFACE('',#10245,23.749,3.175);
#238=TOROIDAL_SURFACE('',#10313,21.209,3.175);
#239=TOROIDAL_SURFACE('',#10509,4.4323,0.508);
#240=TOROIDAL_SURFACE('',#10515,3.4163,0.507999999999992);
#241=TOROIDAL_SURFACE('',#10550,8.52204264558423,1.143);
#242=TOROIDAL_SURFACE('',#10561,18.5282252464232,1.5748);
#243=TOROIDAL_SURFACE('',#10567,18.4629769854638,0.7874);
#244=TOROIDAL_SURFACE('',#10571,13.4366,5.1308);
#245=TOROIDAL_SURFACE('',#10574,13.3900187959915,5.1308);
#246=TOROIDAL_SURFACE('',#10582,6.5656627838263,1.143);
#247=TOROIDAL_SURFACE('',#10585,13.6779,3.3528);
#248=TOROIDAL_SURFACE('',#10636,5.2959,0.762);
#249=TOROIDAL_SURFACE('',#10650,3.8862,0.3175);
#250=TOROIDAL_SURFACE('',#10658,6.06425,0.508);
#251=TOROIDAL_SURFACE('',#10667,6.0071,0.508);
#252=TOROIDAL_SURFACE('',#10684,16.6624,2.413127);
#253=TOROIDAL_SURFACE('',#10688,16.6624,3.429);
#254=TOROIDAL_SURFACE('',#10695,8.89,0.8001);
#255=TOROIDAL_SURFACE('',#10701,16.6624,3.429);
#256=TOROIDAL_SURFACE('',#10704,22.296392545256,3.302);
#257=TOROIDAL_SURFACE('',#10707,23.7562339422346,3.302);
#258=TOROIDAL_SURFACE('',#10711,16.6624,6.477);
#259=TOROIDAL_SURFACE('',#10718,8.0899,1.6002);
#260=TOROIDAL_SURFACE('',#10743,42.00525,3.302);
#261=TOROIDAL_SURFACE('',#10749,42.00525,3.302);
#262=TOROIDAL_SURFACE('',#10776,42.00525,3.302);
#263=TOROIDAL_SURFACE('',#10782,42.00525,3.302);
#264=TOROIDAL_SURFACE('',#10788,42.8625,1.5875);
#265=TOROIDAL_SURFACE('',#10796,48.8219771717602,1.5875);
#266=TOROIDAL_SURFACE('',#10805,48.8219771717602,1.5875);
#267=TOROIDAL_SURFACE('',#10810,42.8625,1.5875);
#268=ELLIPSE('',#10059,8.64513309637285,4.00000000000059);
#269=ELLIPSE('',#10060,8.53586336233429,3.99999999999978);
#270=ELLIPSE('',#10073,2.16128327409315,1.00000000000008);
#271=ELLIPSE('',#10074,2.1339658405822,0.999999999999361);
#272=ELLIPSE('',#10126,8.64513309637285,4.00000000000059);
#273=ELLIPSE('',#10127,8.53586336233429,3.99999999999978);
#274=ELLIPSE('',#10140,2.1339658405822,0.999999999999361);
#275=ELLIPSE('',#10141,2.16128327409315,1.00000000000008);
#276=ELLIPSE('',#10249,40.2698630235017,26.9240000000072);
#277=ELLIPSE('',#10250,78.7205096699893,26.924);
#278=ELLIPSE('',#10252,78.7205096699809,26.924);
#279=ELLIPSE('',#10254,78.7205096699934,26.924);
#280=ELLIPSE('',#10256,78.7205096699875,26.924);
#281=ELLIPSE('',#10258,78.8274961397584,26.989875706612);
#282=ELLIPSE('',#10260,78.7205096699845,26.924);
#283=ELLIPSE('',#10264,78.720509669993,26.924);
#284=ELLIPSE('',#10266,78.7205096699898,26.924);
#285=ELLIPSE('',#10271,78.7161327104488,26.9212320222374);
#286=ELLIPSE('',#10275,78.7205096700008,26.924);
#287=ELLIPSE('',#10279,78.7311209966973,26.9307717285817);
#288=ELLIPSE('',#10286,78.7188049981123,26.9228503591487);
#289=ELLIPSE('',#10288,79.229419439203,27.27149384103);
#290=ELLIPSE('',#10290,78.7276412105627,26.9288675089153);
#291=ELLIPSE('',#10294,78.7207080270773,26.9241356884934);
#292=ELLIPSE('',#10296,78.4080663795393,26.7108901403036);
#293=ELLIPSE('',#10298,78.7247555384231,26.9268969795169);
#294=ELLIPSE('',#10317,36.4708193420335,24.384);
#295=ELLIPSE('',#10326,3.33839256195616,3.17499999999951);
#296=ELLIPSE('',#10327,3.33839256195645,3.175);
#297=ELLIPSE('',#10328,3.33839256195637,3.17499999999995);
#298=ELLIPSE('',#10329,3.33839256195637,3.17499999999984);
#299=ELLIPSE('',#10349,76.2377373734316,26.0723652630412);
#300=ELLIPSE('',#10354,76.2512719263556,26.0815460749879);
#301=ELLIPSE('',#10358,76.3230312814453,26.1304388754083);
#302=ELLIPSE('',#10363,76.2431345257403,26.0760454712399);
#303=ELLIPSE('',#10367,76.2455369777596,26.0776855420129);
#304=ELLIPSE('',#10371,76.2177507943156,26.0587027925807);
#305=ELLIPSE('',#10421,76.2474737169336,26.0788900756951);
#306=ELLIPSE('',#10432,76.2450219445293,26.0773333333334);
#307=ELLIPSE('',#10436,76.2496849526081,26.0802684575528);
#308=ELLIPSE('',#10448,76.2450219445182,26.0773333333334);
#309=ELLIPSE('',#10452,76.24502194451,26.0773333333334);
#310=ELLIPSE('',#10457,76.2450219445164,26.0773333333334);
#311=ELLIPSE('',#10461,76.2324637060495,26.069655541072);
#312=ELLIPSE('',#10463,76.2450219445221,26.0773333333334);
#313=ELLIPSE('',#10470,76.2450219445186,26.0773333333334);
#314=ELLIPSE('',#10497,76.2450219445134,26.0773333333334);
#315=SHAPE_REPRESENTATION_RELATIONSHIP('SRR','None',#18071,#331);
#316=SHAPE_REPRESENTATION_RELATIONSHIP('SRR','None',#18072,#332);
#317=SHAPE_REPRESENTATION_RELATIONSHIP('SRR','None',#18073,#333);
#318=SHAPE_REPRESENTATION_RELATIONSHIP('SRR','None',#18074,#334);
#319=SHAPE_REPRESENTATION_RELATIONSHIP('SRR','None',#18075,#335);
#320=SHAPE_REPRESENTATION_RELATIONSHIP('SRR','None',#18076,#336);
#321=SHAPE_REPRESENTATION_RELATIONSHIP('SRR','None',#18079,#337);
#322=SHAPE_REPRESENTATION_RELATIONSHIP('SRR','None',#18080,#338);
#323=SHAPE_REPRESENTATION_RELATIONSHIP('SRR','None',#18081,#339);
#324=SHAPE_REPRESENTATION_RELATIONSHIP('SRR','None',#18082,#340);
#325=SHAPE_REPRESENTATION_RELATIONSHIP('SRR','None',#18083,#341);
#326=SHAPE_REPRESENTATION_RELATIONSHIP('SRR','None',#18084,#342);
#327=SHAPE_REPRESENTATION_RELATIONSHIP('SRR','None',#18085,#343);
#328=SHAPE_REPRESENTATION_RELATIONSHIP('SRR','None',#18086,#344);
#329=SHAPE_REPRESENTATION_RELATIONSHIP('SRR','None',#18087,#345);
#330=SHAPE_REPRESENTATION_RELATIONSHIP('SRR','None',#18088,#346);
#331=ADVANCED_BREP_SHAPE_REPRESENTATION('',(#363),#17988);
#332=ADVANCED_BREP_SHAPE_REPRESENTATION('',(#364),#17989);
#333=ADVANCED_BREP_SHAPE_REPRESENTATION('',(#365),#17990);
#334=ADVANCED_BREP_SHAPE_REPRESENTATION('',(#366),#17991);
#335=ADVANCED_BREP_SHAPE_REPRESENTATION('',(#367),#17992);
#336=ADVANCED_BREP_SHAPE_REPRESENTATION('',(#368),#17993);
#337=ADVANCED_BREP_SHAPE_REPRESENTATION('',(#369),#17996);
#338=ADVANCED_BREP_SHAPE_REPRESENTATION('',(#370),#17997);
#339=ADVANCED_BREP_SHAPE_REPRESENTATION('',(#371),#17998);
#340=ADVANCED_BREP_SHAPE_REPRESENTATION('',(#372),#17999);
#341=ADVANCED_BREP_SHAPE_REPRESENTATION('',(#373),#18000);
#342=ADVANCED_BREP_SHAPE_REPRESENTATION('',(#374),#18001);
#343=ADVANCED_BREP_SHAPE_REPRESENTATION('',(#375),#18002);
#344=ADVANCED_BREP_SHAPE_REPRESENTATION('',(#376),#18003);
#345=ADVANCED_BREP_SHAPE_REPRESENTATION('',(#377),#18004);
#346=ADVANCED_BREP_SHAPE_REPRESENTATION('',(#378),#18005);
#347=STYLED_ITEM('',(#18170),#363);
#348=STYLED_ITEM('',(#18170),#364);
#349=STYLED_ITEM('',(#18170),#365);
#350=STYLED_ITEM('',(#18171),#366);
#351=STYLED_ITEM('',(#18172),#367);
#352=STYLED_ITEM('',(#18170),#368);
#353=STYLED_ITEM('',(#18172),#369);
#354=STYLED_ITEM('',(#18171),#370);
#355=STYLED_ITEM('',(#18172),#371);
#356=STYLED_ITEM('',(#18172),#372);
#357=STYLED_ITEM('',(#18170),#373);
#358=STYLED_ITEM('',(#18172),#374);
#359=STYLED_ITEM('',(#18170),#375);
#360=STYLED_ITEM('',(#18172),#376);
#361=STYLED_ITEM('',(#18171),#377);
#362=STYLED_ITEM('',(#18171),#378);
#363=MANIFOLD_SOLID_BREP('Body1',#9556);
#364=MANIFOLD_SOLID_BREP('Body1',#9557);
#365=MANIFOLD_SOLID_BREP('Body1',#9558);
#366=MANIFOLD_SOLID_BREP('Body1',#9559);
#367=MANIFOLD_SOLID_BREP('Body1',#9560);
#368=MANIFOLD_SOLID_BREP('Body1',#9561);
#369=MANIFOLD_SOLID_BREP('Body1',#9562);
#370=MANIFOLD_SOLID_BREP('Body1',#9563);
#371=MANIFOLD_SOLID_BREP('Body1',#9564);
#372=MANIFOLD_SOLID_BREP('Body1',#9565);
#373=MANIFOLD_SOLID_BREP('Body1',#9566);
#374=MANIFOLD_SOLID_BREP('Body1',#9567);
#375=MANIFOLD_SOLID_BREP('Body1',#9568);
#376=MANIFOLD_SOLID_BREP('Body1',#9569);
#377=MANIFOLD_SOLID_BREP('Body1',#9570);
#378=MANIFOLD_SOLID_BREP('Body1',#9571);
#379=FACE_BOUND('',#1453,.T.);
#380=FACE_BOUND('',#1454,.T.);
#381=FACE_BOUND('',#1455,.T.);
#382=FACE_BOUND('',#1456,.T.);
#383=FACE_BOUND('',#1459,.T.);
#384=FACE_BOUND('',#1460,.T.);
#385=FACE_BOUND('',#1461,.T.);
#386=FACE_BOUND('',#1462,.T.);
#387=FACE_BOUND('',#1472,.T.);
#388=FACE_BOUND('',#1473,.T.);
#389=FACE_BOUND('',#1474,.T.);
#390=FACE_BOUND('',#1477,.T.);
#391=FACE_BOUND('',#1478,.T.);
#392=FACE_BOUND('',#1479,.T.);
#393=FACE_BOUND('',#1497,.T.);
#394=FACE_BOUND('',#1498,.T.);
#395=FACE_BOUND('',#1500,.T.);
#396=FACE_BOUND('',#1501,.T.);
#397=FACE_BOUND('',#1512,.T.);
#398=FACE_BOUND('',#1513,.T.);
#399=FACE_BOUND('',#1515,.T.);
#400=FACE_BOUND('',#1516,.T.);
#401=FACE_BOUND('',#1553,.T.);
#402=FACE_BOUND('',#1554,.T.);
#403=FACE_BOUND('',#1557,.T.);
#404=FACE_BOUND('',#1558,.T.);
#405=FACE_BOUND('',#1568,.T.);
#406=FACE_BOUND('',#1569,.T.);
#407=FACE_BOUND('',#1572,.T.);
#408=FACE_BOUND('',#1573,.T.);
#409=FACE_BOUND('',#1591,.T.);
#410=FACE_BOUND('',#1592,.T.);
#411=FACE_BOUND('',#1594,.T.);
#412=FACE_BOUND('',#1595,.T.);
#413=FACE_BOUND('',#1606,.T.);
#414=FACE_BOUND('',#1607,.T.);
#415=FACE_BOUND('',#1609,.T.);
#416=FACE_BOUND('',#1610,.T.);
#417=FACE_BOUND('',#1638,.T.);
#418=FACE_BOUND('',#1639,.T.);
#419=FACE_BOUND('',#1640,.T.);
#420=FACE_BOUND('',#1641,.T.);
#421=FACE_BOUND('',#1644,.T.);
#422=FACE_BOUND('',#1645,.T.);
#423=FACE_BOUND('',#1646,.T.);
#424=FACE_BOUND('',#1647,.T.);
#425=FACE_BOUND('',#1650,.T.);
#426=FACE_BOUND('',#1651,.T.);
#427=FACE_BOUND('',#1652,.T.);
#428=FACE_BOUND('',#1653,.T.);
#429=FACE_BOUND('',#1656,.T.);
#430=FACE_BOUND('',#1657,.T.);
#431=FACE_BOUND('',#1658,.T.);
#432=FACE_BOUND('',#1659,.T.);
#433=FACE_BOUND('',#1692,.T.);
#434=FACE_BOUND('',#1693,.T.);
#435=FACE_BOUND('',#1694,.T.);
#436=FACE_BOUND('',#1695,.T.);
#437=FACE_BOUND('',#1698,.T.);
#438=FACE_BOUND('',#1699,.T.);
#439=FACE_BOUND('',#1700,.T.);
#440=FACE_BOUND('',#1701,.T.);
#441=FACE_BOUND('',#1704,.T.);
#442=FACE_BOUND('',#1705,.T.);
#443=FACE_BOUND('',#1706,.T.);
#444=FACE_BOUND('',#1707,.T.);
#445=FACE_BOUND('',#1710,.T.);
#446=FACE_BOUND('',#1711,.T.);
#447=FACE_BOUND('',#1712,.T.);
#448=FACE_BOUND('',#1713,.T.);
#449=FACE_BOUND('',#1749,.T.);
#450=FACE_BOUND('',#1750,.T.);
#451=FACE_BOUND('',#1751,.T.);
#452=FACE_BOUND('',#1754,.T.);
#453=FACE_BOUND('',#1755,.T.);
#454=FACE_BOUND('',#1756,.T.);
#455=FACE_BOUND('',#1793,.T.);
#456=FACE_BOUND('',#1794,.T.);
#457=FACE_BOUND('',#1795,.T.);
#458=FACE_BOUND('',#1796,.T.);
#459=FACE_BOUND('',#1797,.T.);
#460=FACE_BOUND('',#1798,.T.);
#461=FACE_BOUND('',#1819,.T.);
#462=FACE_BOUND('',#1825,.T.);
#463=FACE_BOUND('',#1827,.T.);
#464=FACE_BOUND('',#1829,.T.);
#465=FACE_BOUND('',#1863,.T.);
#466=FACE_BOUND('',#1920,.T.);
#467=FACE_BOUND('',#1929,.T.);
#468=FACE_BOUND('',#1931,.T.);
#469=FACE_BOUND('',#1952,.T.);
#470=FACE_BOUND('',#1954,.T.);
#471=FACE_BOUND('',#1968,.T.);
#472=FACE_BOUND('',#1970,.T.);
#473=FACE_BOUND('',#1972,.T.);
#474=FACE_BOUND('',#1974,.T.);
#475=FACE_BOUND('',#1976,.T.);
#476=FACE_BOUND('',#1983,.T.);
#477=FACE_BOUND('',#1996,.T.);
#478=FACE_BOUND('',#2020,.T.);
#479=FACE_BOUND('',#2022,.T.);
#480=FACE_BOUND('',#2024,.T.);
#481=FACE_BOUND('',#2027,.T.);
#482=FACE_BOUND('',#2048,.T.);
#483=FACE_BOUND('',#2050,.T.);
#484=FACE_BOUND('',#2052,.T.);
#485=FACE_BOUND('',#2054,.T.);
#486=FACE_BOUND('',#2066,.T.);
#487=FACE_BOUND('',#2068,.T.);
#488=FACE_BOUND('',#2070,.T.);
#489=FACE_BOUND('',#2072,.T.);
#490=FACE_BOUND('',#2074,.T.);
#491=FACE_BOUND('',#2076,.T.);
#492=FACE_BOUND('',#2078,.T.);
#493=FACE_BOUND('',#2080,.T.);
#494=FACE_BOUND('',#2095,.T.);
#495=FACE_BOUND('',#2097,.T.);
#496=FACE_BOUND('',#2099,.T.);
#497=FACE_BOUND('',#2101,.T.);
#498=FACE_BOUND('',#2105,.T.);
#499=FACE_BOUND('',#2107,.T.);
#500=FACE_BOUND('',#2113,.T.);
#501=FACE_BOUND('',#2115,.T.);
#502=PLANE('',#9784);
#503=PLANE('',#9786);
#504=PLANE('',#9788);
#505=PLANE('',#9789);
#506=PLANE('',#9790);
#507=PLANE('',#9792);
#508=PLANE('',#9794);
#509=PLANE('',#9797);
#510=PLANE('',#9798);
#511=PLANE('',#9801);
#512=PLANE('',#9802);
#513=PLANE('',#9805);
#514=PLANE('',#9806);
#515=PLANE('',#9809);
#516=PLANE('',#9810);
#517=PLANE('',#9813);
#518=PLANE('',#9816);
#519=PLANE('',#9817);
#520=PLANE('',#9820);
#521=PLANE('',#9821);
#522=PLANE('',#9824);
#523=PLANE('',#9827);
#524=PLANE('',#9828);
#525=PLANE('',#9831);
#526=PLANE('',#9832);
#527=PLANE('',#9833);
#528=PLANE('',#9834);
#529=PLANE('',#9836);
#530=PLANE('',#9839);
#531=PLANE('',#9841);
#532=PLANE('',#9843);
#533=PLANE('',#9844);
#534=PLANE('',#9845);
#535=PLANE('',#9847);
#536=PLANE('',#9849);
#537=PLANE('',#9852);
#538=PLANE('',#9854);
#539=PLANE('',#9855);
#540=PLANE('',#9856);
#541=PLANE('',#9859);
#542=PLANE('',#9864);
#543=PLANE('',#9865);
#544=PLANE('',#9866);
#545=PLANE('',#9867);
#546=PLANE('',#9868);
#547=PLANE('',#9869);
#548=PLANE('',#9870);
#549=PLANE('',#9871);
#550=PLANE('',#9874);
#551=PLANE('',#9879);
#552=PLANE('',#9880);
#553=PLANE('',#9881);
#554=PLANE('',#9882);
#555=PLANE('',#9883);
#556=PLANE('',#9884);
#557=PLANE('',#9885);
#558=PLANE('',#9911);
#559=PLANE('',#9913);
#560=PLANE('',#9915);
#561=PLANE('',#9916);
#562=PLANE('',#9917);
#563=PLANE('',#9919);
#564=PLANE('',#9921);
#565=PLANE('',#9924);
#566=PLANE('',#9925);
#567=PLANE('',#9928);
#568=PLANE('',#9929);
#569=PLANE('',#9932);
#570=PLANE('',#9935);
#571=PLANE('',#9936);
#572=PLANE('',#9939);
#573=PLANE('',#9940);
#574=PLANE('',#9943);
#575=PLANE('',#9946);
#576=PLANE('',#9947);
#577=PLANE('',#9950);
#578=PLANE('',#9951);
#579=PLANE('',#9954);
#580=PLANE('',#9955);
#581=PLANE('',#9958);
#582=PLANE('',#9959);
#583=PLANE('',#9960);
#584=PLANE('',#9961);
#585=PLANE('',#9963);
#586=PLANE('',#9965);
#587=PLANE('',#9968);
#588=PLANE('',#9970);
#589=PLANE('',#9971);
#590=PLANE('',#9972);
#591=PLANE('',#9974);
#592=PLANE('',#9977);
#593=PLANE('',#9979);
#594=PLANE('',#9981);
#595=PLANE('',#9982);
#596=PLANE('',#9983);
#597=PLANE('',#9986);
#598=PLANE('',#9991);
#599=PLANE('',#9992);
#600=PLANE('',#9993);
#601=PLANE('',#9994);
#602=PLANE('',#9995);
#603=PLANE('',#9996);
#604=PLANE('',#9997);
#605=PLANE('',#9998);
#606=PLANE('',#10001);
#607=PLANE('',#10006);
#608=PLANE('',#10007);
#609=PLANE('',#10008);
#610=PLANE('',#10009);
#611=PLANE('',#10010);
#612=PLANE('',#10011);
#613=PLANE('',#10012);
#614=PLANE('',#10038);
#615=PLANE('',#10039);
#616=PLANE('',#10042);
#617=PLANE('',#10043);
#618=PLANE('',#10046);
#619=PLANE('',#10047);
#620=PLANE('',#10050);
#621=PLANE('',#10051);
#622=PLANE('',#10054);
#623=PLANE('',#10055);
#624=PLANE('',#10056);
#625=PLANE('',#10057);
#626=PLANE('',#10061);
#627=PLANE('',#10063);
#628=PLANE('',#10065);
#629=PLANE('',#10066);
#630=PLANE('',#10067);
#631=PLANE('',#10069);
#632=PLANE('',#10071);
#633=PLANE('',#10075);
#634=PLANE('',#10076);
#635=PLANE('',#10077);
#636=PLANE('',#10078);
#637=PLANE('',#10079);
#638=PLANE('',#10105);
#639=PLANE('',#10106);
#640=PLANE('',#10109);
#641=PLANE('',#10110);
#642=PLANE('',#10113);
#643=PLANE('',#10114);
#644=PLANE('',#10117);
#645=PLANE('',#10118);
#646=PLANE('',#10121);
#647=PLANE('',#10122);
#648=PLANE('',#10123);
#649=PLANE('',#10124);
#650=PLANE('',#10128);
#651=PLANE('',#10130);
#652=PLANE('',#10132);
#653=PLANE('',#10133);
#654=PLANE('',#10134);
#655=PLANE('',#10136);
#656=PLANE('',#10138);
#657=PLANE('',#10142);
#658=PLANE('',#10143);
#659=PLANE('',#10144);
#660=PLANE('',#10145);
#661=PLANE('',#10146);
#662=PLANE('',#10157);
#663=PLANE('',#10160);
#664=PLANE('',#10161);
#665=PLANE('',#10164);
#666=PLANE('',#10165);
#667=PLANE('',#10168);
#668=PLANE('',#10169);
#669=PLANE('',#10172);
#670=PLANE('',#10173);
#671=PLANE('',#10176);
#672=PLANE('',#10177);
#673=PLANE('',#10180);
#674=PLANE('',#10181);
#675=PLANE('',#10182);
#676=PLANE('',#10183);
#677=PLANE('',#10184);
#678=PLANE('',#10188);
#679=PLANE('',#10190);
#680=PLANE('',#10192);
#681=PLANE('',#10194);
#682=PLANE('',#10195);
#683=PLANE('',#10196);
#684=PLANE('',#10198);
#685=PLANE('',#10200);
#686=PLANE('',#10202);
#687=PLANE('',#10206);
#688=PLANE('',#10207);
#689=PLANE('',#10208);
#690=PLANE('',#10209);
#691=PLANE('',#10210);
#692=PLANE('',#10212);
#693=PLANE('',#10215);
#694=PLANE('',#10216);
#695=PLANE('',#10219);
#696=PLANE('',#10220);
#697=PLANE('',#10223);
#698=PLANE('',#10224);
#699=PLANE('',#10227);
#700=PLANE('',#10228);
#701=PLANE('',#10229);
#702=PLANE('',#10230);
#703=PLANE('',#10232);
#704=PLANE('',#10234);
#705=PLANE('',#10235);
#706=PLANE('',#10236);
#707=PLANE('',#10238);
#708=PLANE('',#10240);
#709=PLANE('',#10241);
#710=PLANE('',#10324);
#711=PLANE('',#10325);
#712=PLANE('',#10336);
#713=PLANE('',#10341);
#714=PLANE('',#10342);
#715=PLANE('',#10343);
#716=PLANE('',#10345);
#717=PLANE('',#10348);
#718=PLANE('',#10353);
#719=PLANE('',#10355);
#720=PLANE('',#10357);
#721=PLANE('',#10360);
#722=PLANE('',#10362);
#723=PLANE('',#10366);
#724=PLANE('',#10368);
#725=PLANE('',#10370);
#726=PLANE('',#10372);
#727=PLANE('',#10374);
#728=PLANE('',#10376);
#729=PLANE('',#10378);
#730=PLANE('',#10380);
#731=PLANE('',#10382);
#732=PLANE('',#10388);
#733=PLANE('',#10390);
#734=PLANE('',#10392);
#735=PLANE('',#10394);
#736=PLANE('',#10401);
#737=PLANE('',#10403);
#738=PLANE('',#10406);
#739=PLANE('',#10409);
#740=PLANE('',#10416);
#741=PLANE('',#10418);
#742=PLANE('',#10420);
#743=PLANE('',#10423);
#744=PLANE('',#10425);
#745=PLANE('',#10428);
#746=PLANE('',#10431);
#747=PLANE('',#10433);
#748=PLANE('',#10435);
#749=PLANE('',#10437);
#750=PLANE('',#10439);
#751=PLANE('',#10441);
#752=PLANE('',#10447);
#753=PLANE('',#10449);
#754=PLANE('',#10451);
#755=PLANE('',#10454);
#756=PLANE('',#10456);
#757=PLANE('',#10458);
#758=PLANE('',#10460);
#759=PLANE('',#10462);
#760=PLANE('',#10464);
#761=PLANE('',#10466);
#762=PLANE('',#10469);
#763=PLANE('',#10471);
#764=PLANE('',#10473);
#765=PLANE('',#10475);
#766=PLANE('',#10478);
#767=PLANE('',#10482);
#768=PLANE('',#10486);
#769=PLANE('',#10490);
#770=PLANE('',#10499);
#771=PLANE('',#10500);
#772=PLANE('',#10501);
#773=PLANE('',#10502);
#774=PLANE('',#10506);
#775=PLANE('',#10507);
#776=PLANE('',#10526);
#777=PLANE('',#10537);
#778=PLANE('',#10538);
#779=PLANE('',#10539);
#780=PLANE('',#10540);
#781=PLANE('',#10541);
#782=PLANE('',#10542);
#783=PLANE('',#10543);
#784=PLANE('',#10544);
#785=PLANE('',#10545);
#786=PLANE('',#10587);
#787=PLANE('',#10588);
#788=PLANE('',#10589);
#789=PLANE('',#10590);
#790=PLANE('',#10591);
#791=PLANE('',#10611);
#792=PLANE('',#10622);
#793=PLANE('',#10623);
#794=PLANE('',#10624);
#795=PLANE('',#10625);
#796=PLANE('',#10626);
#797=PLANE('',#10627);
#798=PLANE('',#10628);
#799=PLANE('',#10629);
#800=PLANE('',#10630);
#801=PLANE('',#10631);
#802=PLANE('',#10632);
#803=PLANE('',#10633);
#804=PLANE('',#10634);
#805=PLANE('',#10675);
#806=PLANE('',#10676);
#807=PLANE('',#10677);
#808=PLANE('',#10678);
#809=PLANE('',#10679);
#810=PLANE('',#10680);
#811=PLANE('',#10681);
#812=PLANE('',#10682);
#813=PLANE('',#10721);
#814=PLANE('',#10722);
#815=PLANE('',#10723);
#816=PLANE('',#10724);
#817=PLANE('',#10725);
#818=PLANE('',#10726);
#819=PLANE('',#10727);
#820=PLANE('',#10728);
#821=PLANE('',#10729);
#822=PLANE('',#10730);
#823=PLANE('',#10731);
#824=PLANE('',#10732);
#825=PLANE('',#10764);
#826=PLANE('',#10765);
#827=PLANE('',#10766);
#828=PLANE('',#10767);
#829=PLANE('',#10768);
#830=PLANE('',#10769);
#831=PLANE('',#10770);
#832=PLANE('',#10771);
#833=PLANE('',#10813);
#834=PLANE('',#10814);
#835=PLANE('',#10815);
#836=PLANE('',#10816);
#837=PLANE('',#10824);
#838=PLANE('',#10825);
#839=PLANE('',#10838);
#840=PLANE('',#10839);
#841=FACE_OUTER_BOUND('',#1417,.T.);
#842=FACE_OUTER_BOUND('',#1418,.T.);
#843=FACE_OUTER_BOUND('',#1419,.T.);
#844=FACE_OUTER_BOUND('',#1420,.T.);
#845=FACE_OUTER_BOUND('',#1421,.T.);
#846=FACE_OUTER_BOUND('',#1422,.T.);
#847=FACE_OUTER_BOUND('',#1423,.T.);
#848=FACE_OUTER_BOUND('',#1424,.T.);
#849=FACE_OUTER_BOUND('',#1425,.T.);
#850=FACE_OUTER_BOUND('',#1426,.T.);
#851=FACE_OUTER_BOUND('',#1427,.T.);
#852=FACE_OUTER_BOUND('',#1428,.T.);
#853=FACE_OUTER_BOUND('',#1429,.T.);
#854=FACE_OUTER_BOUND('',#1430,.T.);
#855=FACE_OUTER_BOUND('',#1431,.T.);
#856=FACE_OUTER_BOUND('',#1432,.T.);
#857=FACE_OUTER_BOUND('',#1433,.T.);
#858=FACE_OUTER_BOUND('',#1434,.T.);
#859=FACE_OUTER_BOUND('',#1435,.T.);
#860=FACE_OUTER_BOUND('',#1436,.T.);
#861=FACE_OUTER_BOUND('',#1437,.T.);
#862=FACE_OUTER_BOUND('',#1438,.T.);
#863=FACE_OUTER_BOUND('',#1439,.T.);
#864=FACE_OUTER_BOUND('',#1440,.T.);
#865=FACE_OUTER_BOUND('',#1441,.T.);
#866=FACE_OUTER_BOUND('',#1442,.T.);
#867=FACE_OUTER_BOUND('',#1443,.T.);
#868=FACE_OUTER_BOUND('',#1444,.T.);
#869=FACE_OUTER_BOUND('',#1445,.T.);
#870=FACE_OUTER_BOUND('',#1446,.T.);
#871=FACE_OUTER_BOUND('',#1447,.T.);
#872=FACE_OUTER_BOUND('',#1448,.T.);
#873=FACE_OUTER_BOUND('',#1449,.T.);
#874=FACE_OUTER_BOUND('',#1450,.T.);
#875=FACE_OUTER_BOUND('',#1451,.T.);
#876=FACE_OUTER_BOUND('',#1452,.T.);
#877=FACE_OUTER_BOUND('',#1457,.T.);
#878=FACE_OUTER_BOUND('',#1458,.T.);
#879=FACE_OUTER_BOUND('',#1463,.T.);
#880=FACE_OUTER_BOUND('',#1464,.T.);
#881=FACE_OUTER_BOUND('',#1465,.T.);
#882=FACE_OUTER_BOUND('',#1466,.T.);
#883=FACE_OUTER_BOUND('',#1467,.T.);
#884=FACE_OUTER_BOUND('',#1468,.T.);
#885=FACE_OUTER_BOUND('',#1469,.T.);
#886=FACE_OUTER_BOUND('',#1470,.T.);
#887=FACE_OUTER_BOUND('',#1471,.T.);
#888=FACE_OUTER_BOUND('',#1475,.T.);
#889=FACE_OUTER_BOUND('',#1476,.T.);
#890=FACE_OUTER_BOUND('',#1480,.T.);
#891=FACE_OUTER_BOUND('',#1481,.T.);
#892=FACE_OUTER_BOUND('',#1482,.T.);
#893=FACE_OUTER_BOUND('',#1483,.T.);
#894=FACE_OUTER_BOUND('',#1484,.T.);
#895=FACE_OUTER_BOUND('',#1485,.T.);
#896=FACE_OUTER_BOUND('',#1486,.T.);
#897=FACE_OUTER_BOUND('',#1487,.T.);
#898=FACE_OUTER_BOUND('',#1488,.T.);
#899=FACE_OUTER_BOUND('',#1489,.T.);
#900=FACE_OUTER_BOUND('',#1490,.T.);
#901=FACE_OUTER_BOUND('',#1491,.T.);
#902=FACE_OUTER_BOUND('',#1492,.T.);
#903=FACE_OUTER_BOUND('',#1493,.T.);
#904=FACE_OUTER_BOUND('',#1494,.T.);
#905=FACE_OUTER_BOUND('',#1495,.T.);
#906=FACE_OUTER_BOUND('',#1496,.T.);
#907=FACE_OUTER_BOUND('',#1499,.T.);
#908=FACE_OUTER_BOUND('',#1502,.T.);
#909=FACE_OUTER_BOUND('',#1503,.T.);
#910=FACE_OUTER_BOUND('',#1504,.T.);
#911=FACE_OUTER_BOUND('',#1505,.T.);
#912=FACE_OUTER_BOUND('',#1506,.T.);
#913=FACE_OUTER_BOUND('',#1507,.T.);
#914=FACE_OUTER_BOUND('',#1508,.T.);
#915=FACE_OUTER_BOUND('',#1509,.T.);
#916=FACE_OUTER_BOUND('',#1510,.T.);
#917=FACE_OUTER_BOUND('',#1511,.T.);
#918=FACE_OUTER_BOUND('',#1514,.T.);
#919=FACE_OUTER_BOUND('',#1517,.T.);
#920=FACE_OUTER_BOUND('',#1518,.T.);
#921=FACE_OUTER_BOUND('',#1519,.T.);
#922=FACE_OUTER_BOUND('',#1520,.T.);
#923=FACE_OUTER_BOUND('',#1521,.T.);
#924=FACE_OUTER_BOUND('',#1522,.T.);
#925=FACE_OUTER_BOUND('',#1523,.T.);
#926=FACE_OUTER_BOUND('',#1524,.T.);
#927=FACE_OUTER_BOUND('',#1525,.T.);
#928=FACE_OUTER_BOUND('',#1526,.T.);
#929=FACE_OUTER_BOUND('',#1527,.T.);
#930=FACE_OUTER_BOUND('',#1528,.T.);
#931=FACE_OUTER_BOUND('',#1529,.T.);
#932=FACE_OUTER_BOUND('',#1530,.T.);
#933=FACE_OUTER_BOUND('',#1531,.T.);
#934=FACE_OUTER_BOUND('',#1532,.T.);
#935=FACE_OUTER_BOUND('',#1533,.T.);
#936=FACE_OUTER_BOUND('',#1534,.T.);
#937=FACE_OUTER_BOUND('',#1535,.T.);
#938=FACE_OUTER_BOUND('',#1536,.T.);
#939=FACE_OUTER_BOUND('',#1537,.T.);
#940=FACE_OUTER_BOUND('',#1538,.T.);
#941=FACE_OUTER_BOUND('',#1539,.T.);
#942=FACE_OUTER_BOUND('',#1540,.T.);
#943=FACE_OUTER_BOUND('',#1541,.T.);
#944=FACE_OUTER_BOUND('',#1542,.T.);
#945=FACE_OUTER_BOUND('',#1543,.T.);
#946=FACE_OUTER_BOUND('',#1544,.T.);
#947=FACE_OUTER_BOUND('',#1545,.T.);
#948=FACE_OUTER_BOUND('',#1546,.T.);
#949=FACE_OUTER_BOUND('',#1547,.T.);
#950=FACE_OUTER_BOUND('',#1548,.T.);
#951=FACE_OUTER_BOUND('',#1549,.T.);
#952=FACE_OUTER_BOUND('',#1550,.T.);
#953=FACE_OUTER_BOUND('',#1551,.T.);
#954=FACE_OUTER_BOUND('',#1552,.T.);
#955=FACE_OUTER_BOUND('',#1555,.T.);
#956=FACE_OUTER_BOUND('',#1556,.T.);
#957=FACE_OUTER_BOUND('',#1559,.T.);
#958=FACE_OUTER_BOUND('',#1560,.T.);
#959=FACE_OUTER_BOUND('',#1561,.T.);
#960=FACE_OUTER_BOUND('',#1562,.T.);
#961=FACE_OUTER_BOUND('',#1563,.T.);
#962=FACE_OUTER_BOUND('',#1564,.T.);
#963=FACE_OUTER_BOUND('',#1565,.T.);
#964=FACE_OUTER_BOUND('',#1566,.T.);
#965=FACE_OUTER_BOUND('',#1567,.T.);
#966=FACE_OUTER_BOUND('',#1570,.T.);
#967=FACE_OUTER_BOUND('',#1571,.T.);
#968=FACE_OUTER_BOUND('',#1574,.T.);
#969=FACE_OUTER_BOUND('',#1575,.T.);
#970=FACE_OUTER_BOUND('',#1576,.T.);
#971=FACE_OUTER_BOUND('',#1577,.T.);
#972=FACE_OUTER_BOUND('',#1578,.T.);
#973=FACE_OUTER_BOUND('',#1579,.T.);
#974=FACE_OUTER_BOUND('',#1580,.T.);
#975=FACE_OUTER_BOUND('',#1581,.T.);
#976=FACE_OUTER_BOUND('',#1582,.T.);
#977=FACE_OUTER_BOUND('',#1583,.T.);
#978=FACE_OUTER_BOUND('',#1584,.T.);
#979=FACE_OUTER_BOUND('',#1585,.T.);
#980=FACE_OUTER_BOUND('',#1586,.T.);
#981=FACE_OUTER_BOUND('',#1587,.T.);
#982=FACE_OUTER_BOUND('',#1588,.T.);
#983=FACE_OUTER_BOUND('',#1589,.T.);
#984=FACE_OUTER_BOUND('',#1590,.T.);
#985=FACE_OUTER_BOUND('',#1593,.T.);
#986=FACE_OUTER_BOUND('',#1596,.T.);
#987=FACE_OUTER_BOUND('',#1597,.T.);
#988=FACE_OUTER_BOUND('',#1598,.T.);
#989=FACE_OUTER_BOUND('',#1599,.T.);
#990=FACE_OUTER_BOUND('',#1600,.T.);
#991=FACE_OUTER_BOUND('',#1601,.T.);
#992=FACE_OUTER_BOUND('',#1602,.T.);
#993=FACE_OUTER_BOUND('',#1603,.T.);
#994=FACE_OUTER_BOUND('',#1604,.T.);
#995=FACE_OUTER_BOUND('',#1605,.T.);
#996=FACE_OUTER_BOUND('',#1608,.T.);
#997=FACE_OUTER_BOUND('',#1611,.T.);
#998=FACE_OUTER_BOUND('',#1612,.T.);
#999=FACE_OUTER_BOUND('',#1613,.T.);
#1000=FACE_OUTER_BOUND('',#1614,.T.);
#1001=FACE_OUTER_BOUND('',#1615,.T.);
#1002=FACE_OUTER_BOUND('',#1616,.T.);
#1003=FACE_OUTER_BOUND('',#1617,.T.);
#1004=FACE_OUTER_BOUND('',#1618,.T.);
#1005=FACE_OUTER_BOUND('',#1619,.T.);
#1006=FACE_OUTER_BOUND('',#1620,.T.);
#1007=FACE_OUTER_BOUND('',#1621,.T.);
#1008=FACE_OUTER_BOUND('',#1622,.T.);
#1009=FACE_OUTER_BOUND('',#1623,.T.);
#1010=FACE_OUTER_BOUND('',#1624,.T.);
#1011=FACE_OUTER_BOUND('',#1625,.T.);
#1012=FACE_OUTER_BOUND('',#1626,.T.);
#1013=FACE_OUTER_BOUND('',#1627,.T.);
#1014=FACE_OUTER_BOUND('',#1628,.T.);
#1015=FACE_OUTER_BOUND('',#1629,.T.);
#1016=FACE_OUTER_BOUND('',#1630,.T.);
#1017=FACE_OUTER_BOUND('',#1631,.T.);
#1018=FACE_OUTER_BOUND('',#1632,.T.);
#1019=FACE_OUTER_BOUND('',#1633,.T.);
#1020=FACE_OUTER_BOUND('',#1634,.T.);
#1021=FACE_OUTER_BOUND('',#1635,.T.);
#1022=FACE_OUTER_BOUND('',#1636,.T.);
#1023=FACE_OUTER_BOUND('',#1637,.T.);
#1024=FACE_OUTER_BOUND('',#1642,.T.);
#1025=FACE_OUTER_BOUND('',#1643,.T.);
#1026=FACE_OUTER_BOUND('',#1648,.T.);
#1027=FACE_OUTER_BOUND('',#1649,.T.);
#1028=FACE_OUTER_BOUND('',#1654,.T.);
#1029=FACE_OUTER_BOUND('',#1655,.T.);
#1030=FACE_OUTER_BOUND('',#1660,.T.);
#1031=FACE_OUTER_BOUND('',#1661,.T.);
#1032=FACE_OUTER_BOUND('',#1662,.T.);
#1033=FACE_OUTER_BOUND('',#1663,.T.);
#1034=FACE_OUTER_BOUND('',#1664,.T.);
#1035=FACE_OUTER_BOUND('',#1665,.T.);
#1036=FACE_OUTER_BOUND('',#1666,.T.);
#1037=FACE_OUTER_BOUND('',#1667,.T.);
#1038=FACE_OUTER_BOUND('',#1668,.T.);
#1039=FACE_OUTER_BOUND('',#1669,.T.);
#1040=FACE_OUTER_BOUND('',#1670,.T.);
#1041=FACE_OUTER_BOUND('',#1671,.T.);
#1042=FACE_OUTER_BOUND('',#1672,.T.);
#1043=FACE_OUTER_BOUND('',#1673,.T.);
#1044=FACE_OUTER_BOUND('',#1674,.T.);
#1045=FACE_OUTER_BOUND('',#1675,.T.);
#1046=FACE_OUTER_BOUND('',#1676,.T.);
#1047=FACE_OUTER_BOUND('',#1677,.T.);
#1048=FACE_OUTER_BOUND('',#1678,.T.);
#1049=FACE_OUTER_BOUND('',#1679,.T.);
#1050=FACE_OUTER_BOUND('',#1680,.T.);
#1051=FACE_OUTER_BOUND('',#1681,.T.);
#1052=FACE_OUTER_BOUND('',#1682,.T.);
#1053=FACE_OUTER_BOUND('',#1683,.T.);
#1054=FACE_OUTER_BOUND('',#1684,.T.);
#1055=FACE_OUTER_BOUND('',#1685,.T.);
#1056=FACE_OUTER_BOUND('',#1686,.T.);
#1057=FACE_OUTER_BOUND('',#1687,.T.);
#1058=FACE_OUTER_BOUND('',#1688,.T.);
#1059=FACE_OUTER_BOUND('',#1689,.T.);
#1060=FACE_OUTER_BOUND('',#1690,.T.);
#1061=FACE_OUTER_BOUND('',#1691,.T.);
#1062=FACE_OUTER_BOUND('',#1696,.T.);
#1063=FACE_OUTER_BOUND('',#1697,.T.);
#1064=FACE_OUTER_BOUND('',#1702,.T.);
#1065=FACE_OUTER_BOUND('',#1703,.T.);
#1066=FACE_OUTER_BOUND('',#1708,.T.);
#1067=FACE_OUTER_BOUND('',#1709,.T.);
#1068=FACE_OUTER_BOUND('',#1714,.T.);
#1069=FACE_OUTER_BOUND('',#1715,.T.);
#1070=FACE_OUTER_BOUND('',#1716,.T.);
#1071=FACE_OUTER_BOUND('',#1717,.T.);
#1072=FACE_OUTER_BOUND('',#1718,.T.);
#1073=FACE_OUTER_BOUND('',#1719,.T.);
#1074=FACE_OUTER_BOUND('',#1720,.T.);
#1075=FACE_OUTER_BOUND('',#1721,.T.);
#1076=FACE_OUTER_BOUND('',#1722,.T.);
#1077=FACE_OUTER_BOUND('',#1723,.T.);
#1078=FACE_OUTER_BOUND('',#1724,.T.);
#1079=FACE_OUTER_BOUND('',#1725,.T.);
#1080=FACE_OUTER_BOUND('',#1726,.T.);
#1081=FACE_OUTER_BOUND('',#1727,.T.);
#1082=FACE_OUTER_BOUND('',#1728,.T.);
#1083=FACE_OUTER_BOUND('',#1729,.T.);
#1084=FACE_OUTER_BOUND('',#1730,.T.);
#1085=FACE_OUTER_BOUND('',#1731,.T.);
#1086=FACE_OUTER_BOUND('',#1732,.T.);
#1087=FACE_OUTER_BOUND('',#1733,.T.);
#1088=FACE_OUTER_BOUND('',#1734,.T.);
#1089=FACE_OUTER_BOUND('',#1735,.T.);
#1090=FACE_OUTER_BOUND('',#1736,.T.);
#1091=FACE_OUTER_BOUND('',#1737,.T.);
#1092=FACE_OUTER_BOUND('',#1738,.T.);
#1093=FACE_OUTER_BOUND('',#1739,.T.);
#1094=FACE_OUTER_BOUND('',#1740,.T.);
#1095=FACE_OUTER_BOUND('',#1741,.T.);
#1096=FACE_OUTER_BOUND('',#1742,.T.);
#1097=FACE_OUTER_BOUND('',#1743,.T.);
#1098=FACE_OUTER_BOUND('',#1744,.T.);
#1099=FACE_OUTER_BOUND('',#1745,.T.);
#1100=FACE_OUTER_BOUND('',#1746,.T.);
#1101=FACE_OUTER_BOUND('',#1747,.T.);
#1102=FACE_OUTER_BOUND('',#1748,.T.);
#1103=FACE_OUTER_BOUND('',#1752,.T.);
#1104=FACE_OUTER_BOUND('',#1753,.T.);
#1105=FACE_OUTER_BOUND('',#1757,.T.);
#1106=FACE_OUTER_BOUND('',#1758,.T.);
#1107=FACE_OUTER_BOUND('',#1759,.T.);
#1108=FACE_OUTER_BOUND('',#1760,.T.);
#1109=FACE_OUTER_BOUND('',#1761,.T.);
#1110=FACE_OUTER_BOUND('',#1762,.T.);
#1111=FACE_OUTER_BOUND('',#1763,.T.);
#1112=FACE_OUTER_BOUND('',#1764,.T.);
#1113=FACE_OUTER_BOUND('',#1765,.T.);
#1114=FACE_OUTER_BOUND('',#1766,.T.);
#1115=FACE_OUTER_BOUND('',#1767,.T.);
#1116=FACE_OUTER_BOUND('',#1768,.T.);
#1117=FACE_OUTER_BOUND('',#1769,.T.);
#1118=FACE_OUTER_BOUND('',#1770,.T.);
#1119=FACE_OUTER_BOUND('',#1771,.T.);
#1120=FACE_OUTER_BOUND('',#1772,.T.);
#1121=FACE_OUTER_BOUND('',#1773,.T.);
#1122=FACE_OUTER_BOUND('',#1774,.T.);
#1123=FACE_OUTER_BOUND('',#1775,.T.);
#1124=FACE_OUTER_BOUND('',#1776,.T.);
#1125=FACE_OUTER_BOUND('',#1777,.T.);
#1126=FACE_OUTER_BOUND('',#1778,.T.);
#1127=FACE_OUTER_BOUND('',#1779,.T.);
#1128=FACE_OUTER_BOUND('',#1780,.T.);
#1129=FACE_OUTER_BOUND('',#1781,.T.);
#1130=FACE_OUTER_BOUND('',#1782,.T.);
#1131=FACE_OUTER_BOUND('',#1783,.T.);
#1132=FACE_OUTER_BOUND('',#1784,.T.);
#1133=FACE_OUTER_BOUND('',#1785,.T.);
#1134=FACE_OUTER_BOUND('',#1786,.T.);
#1135=FACE_OUTER_BOUND('',#1787,.T.);
#1136=FACE_OUTER_BOUND('',#1788,.T.);
#1137=FACE_OUTER_BOUND('',#1789,.T.);
#1138=FACE_OUTER_BOUND('',#1790,.T.);
#1139=FACE_OUTER_BOUND('',#1791,.T.);
#1140=FACE_OUTER_BOUND('',#1792,.T.);
#1141=FACE_OUTER_BOUND('',#1799,.T.);
#1142=FACE_OUTER_BOUND('',#1800,.T.);
#1143=FACE_OUTER_BOUND('',#1801,.T.);
#1144=FACE_OUTER_BOUND('',#1802,.T.);
#1145=FACE_OUTER_BOUND('',#1803,.T.);
#1146=FACE_OUTER_BOUND('',#1804,.T.);
#1147=FACE_OUTER_BOUND('',#1805,.T.);
#1148=FACE_OUTER_BOUND('',#1806,.T.);
#1149=FACE_OUTER_BOUND('',#1807,.T.);
#1150=FACE_OUTER_BOUND('',#1808,.T.);
#1151=FACE_OUTER_BOUND('',#1809,.T.);
#1152=FACE_OUTER_BOUND('',#1810,.T.);
#1153=FACE_OUTER_BOUND('',#1811,.T.);
#1154=FACE_OUTER_BOUND('',#1812,.T.);
#1155=FACE_OUTER_BOUND('',#1813,.T.);
#1156=FACE_OUTER_BOUND('',#1814,.T.);
#1157=FACE_OUTER_BOUND('',#1815,.T.);
#1158=FACE_OUTER_BOUND('',#1816,.T.);
#1159=FACE_OUTER_BOUND('',#1817,.T.);
#1160=FACE_OUTER_BOUND('',#1818,.T.);
#1161=FACE_OUTER_BOUND('',#1820,.T.);
#1162=FACE_OUTER_BOUND('',#1821,.T.);
#1163=FACE_OUTER_BOUND('',#1822,.T.);
#1164=FACE_OUTER_BOUND('',#1823,.T.);
#1165=FACE_OUTER_BOUND('',#1824,.T.);
#1166=FACE_OUTER_BOUND('',#1826,.T.);
#1167=FACE_OUTER_BOUND('',#1828,.T.);
#1168=FACE_OUTER_BOUND('',#1830,.T.);
#1169=FACE_OUTER_BOUND('',#1831,.T.);
#1170=FACE_OUTER_BOUND('',#1832,.T.);
#1171=FACE_OUTER_BOUND('',#1833,.T.);
#1172=FACE_OUTER_BOUND('',#1834,.T.);
#1173=FACE_OUTER_BOUND('',#1835,.T.);
#1174=FACE_OUTER_BOUND('',#1836,.T.);
#1175=FACE_OUTER_BOUND('',#1837,.T.);
#1176=FACE_OUTER_BOUND('',#1838,.T.);
#1177=FACE_OUTER_BOUND('',#1839,.T.);
#1178=FACE_OUTER_BOUND('',#1840,.T.);
#1179=FACE_OUTER_BOUND('',#1841,.T.);
#1180=FACE_OUTER_BOUND('',#1842,.T.);
#1181=FACE_OUTER_BOUND('',#1843,.T.);
#1182=FACE_OUTER_BOUND('',#1844,.T.);
#1183=FACE_OUTER_BOUND('',#1845,.T.);
#1184=FACE_OUTER_BOUND('',#1846,.T.);
#1185=FACE_OUTER_BOUND('',#1847,.T.);
#1186=FACE_OUTER_BOUND('',#1848,.T.);
#1187=FACE_OUTER_BOUND('',#1849,.T.);
#1188=FACE_OUTER_BOUND('',#1850,.T.);
#1189=FACE_OUTER_BOUND('',#1851,.T.);
#1190=FACE_OUTER_BOUND('',#1852,.T.);
#1191=FACE_OUTER_BOUND('',#1853,.T.);
#1192=FACE_OUTER_BOUND('',#1854,.T.);
#1193=FACE_OUTER_BOUND('',#1855,.T.);
#1194=FACE_OUTER_BOUND('',#1856,.T.);
#1195=FACE_OUTER_BOUND('',#1857,.T.);
#1196=FACE_OUTER_BOUND('',#1858,.T.);
#1197=FACE_OUTER_BOUND('',#1859,.T.);
#1198=FACE_OUTER_BOUND('',#1860,.T.);
#1199=FACE_OUTER_BOUND('',#1861,.T.);
#1200=FACE_OUTER_BOUND('',#1862,.T.);
#1201=FACE_OUTER_BOUND('',#1864,.T.);
#1202=FACE_OUTER_BOUND('',#1865,.T.);
#1203=FACE_OUTER_BOUND('',#1866,.T.);
#1204=FACE_OUTER_BOUND('',#1867,.T.);
#1205=FACE_OUTER_BOUND('',#1868,.T.);
#1206=FACE_OUTER_BOUND('',#1869,.T.);
#1207=FACE_OUTER_BOUND('',#1870,.T.);
#1208=FACE_OUTER_BOUND('',#1871,.T.);
#1209=FACE_OUTER_BOUND('',#1872,.T.);
#1210=FACE_OUTER_BOUND('',#1873,.T.);
#1211=FACE_OUTER_BOUND('',#1874,.T.);
#1212=FACE_OUTER_BOUND('',#1875,.T.);
#1213=FACE_OUTER_BOUND('',#1876,.T.);
#1214=FACE_OUTER_BOUND('',#1877,.T.);
#1215=FACE_OUTER_BOUND('',#1878,.T.);
#1216=FACE_OUTER_BOUND('',#1879,.T.);
#1217=FACE_OUTER_BOUND('',#1880,.T.);
#1218=FACE_OUTER_BOUND('',#1881,.T.);
#1219=FACE_OUTER_BOUND('',#1882,.T.);
#1220=FACE_OUTER_BOUND('',#1883,.T.);
#1221=FACE_OUTER_BOUND('',#1884,.T.);
#1222=FACE_OUTER_BOUND('',#1885,.T.);
#1223=FACE_OUTER_BOUND('',#1886,.T.);
#1224=FACE_OUTER_BOUND('',#1887,.T.);
#1225=FACE_OUTER_BOUND('',#1888,.T.);
#1226=FACE_OUTER_BOUND('',#1889,.T.);
#1227=FACE_OUTER_BOUND('',#1890,.T.);
#1228=FACE_OUTER_BOUND('',#1891,.T.);
#1229=FACE_OUTER_BOUND('',#1892,.T.);
#1230=FACE_OUTER_BOUND('',#1893,.T.);
#1231=FACE_OUTER_BOUND('',#1894,.T.);
#1232=FACE_OUTER_BOUND('',#1895,.T.);
#1233=FACE_OUTER_BOUND('',#1896,.T.);
#1234=FACE_OUTER_BOUND('',#1897,.T.);
#1235=FACE_OUTER_BOUND('',#1898,.T.);
#1236=FACE_OUTER_BOUND('',#1899,.T.);
#1237=FACE_OUTER_BOUND('',#1900,.T.);
#1238=FACE_OUTER_BOUND('',#1901,.T.);
#1239=FACE_OUTER_BOUND('',#1902,.T.);
#1240=FACE_OUTER_BOUND('',#1903,.T.);
#1241=FACE_OUTER_BOUND('',#1904,.T.);
#1242=FACE_OUTER_BOUND('',#1905,.T.);
#1243=FACE_OUTER_BOUND('',#1906,.T.);
#1244=FACE_OUTER_BOUND('',#1907,.T.);
#1245=FACE_OUTER_BOUND('',#1908,.T.);
#1246=FACE_OUTER_BOUND('',#1909,.T.);
#1247=FACE_OUTER_BOUND('',#1910,.T.);
#1248=FACE_OUTER_BOUND('',#1911,.T.);
#1249=FACE_OUTER_BOUND('',#1912,.T.);
#1250=FACE_OUTER_BOUND('',#1913,.T.);
#1251=FACE_OUTER_BOUND('',#1914,.T.);
#1252=FACE_OUTER_BOUND('',#1915,.T.);
#1253=FACE_OUTER_BOUND('',#1916,.T.);
#1254=FACE_OUTER_BOUND('',#1917,.T.);
#1255=FACE_OUTER_BOUND('',#1918,.T.);
#1256=FACE_OUTER_BOUND('',#1919,.T.);
#1257=FACE_OUTER_BOUND('',#1921,.T.);
#1258=FACE_OUTER_BOUND('',#1922,.T.);
#1259=FACE_OUTER_BOUND('',#1923,.T.);
#1260=FACE_OUTER_BOUND('',#1924,.T.);
#1261=FACE_OUTER_BOUND('',#1925,.T.);
#1262=FACE_OUTER_BOUND('',#1926,.T.);
#1263=FACE_OUTER_BOUND('',#1927,.T.);
#1264=FACE_OUTER_BOUND('',#1928,.T.);
#1265=FACE_OUTER_BOUND('',#1930,.T.);
#1266=FACE_OUTER_BOUND('',#1932,.T.);
#1267=FACE_OUTER_BOUND('',#1933,.T.);
#1268=FACE_OUTER_BOUND('',#1934,.T.);
#1269=FACE_OUTER_BOUND('',#1935,.T.);
#1270=FACE_OUTER_BOUND('',#1936,.T.);
#1271=FACE_OUTER_BOUND('',#1937,.T.);
#1272=FACE_OUTER_BOUND('',#1938,.T.);
#1273=FACE_OUTER_BOUND('',#1939,.T.);
#1274=FACE_OUTER_BOUND('',#1940,.T.);
#1275=FACE_OUTER_BOUND('',#1941,.T.);
#1276=FACE_OUTER_BOUND('',#1942,.T.);
#1277=FACE_OUTER_BOUND('',#1943,.T.);
#1278=FACE_OUTER_BOUND('',#1944,.T.);
#1279=FACE_OUTER_BOUND('',#1945,.T.);
#1280=FACE_OUTER_BOUND('',#1946,.T.);
#1281=FACE_OUTER_BOUND('',#1947,.T.);
#1282=FACE_OUTER_BOUND('',#1948,.T.);
#1283=FACE_OUTER_BOUND('',#1949,.T.);
#1284=FACE_OUTER_BOUND('',#1950,.T.);
#1285=FACE_OUTER_BOUND('',#1951,.T.);
#1286=FACE_OUTER_BOUND('',#1953,.T.);
#1287=FACE_OUTER_BOUND('',#1955,.T.);
#1288=FACE_OUTER_BOUND('',#1956,.T.);
#1289=FACE_OUTER_BOUND('',#1957,.T.);
#1290=FACE_OUTER_BOUND('',#1958,.T.);
#1291=FACE_OUTER_BOUND('',#1959,.T.);
#1292=FACE_OUTER_BOUND('',#1960,.T.);
#1293=FACE_OUTER_BOUND('',#1961,.T.);
#1294=FACE_OUTER_BOUND('',#1962,.T.);
#1295=FACE_OUTER_BOUND('',#1963,.T.);
#1296=FACE_OUTER_BOUND('',#1964,.T.);
#1297=FACE_OUTER_BOUND('',#1965,.T.);
#1298=FACE_OUTER_BOUND('',#1966,.T.);
#1299=FACE_OUTER_BOUND('',#1967,.T.);
#1300=FACE_OUTER_BOUND('',#1969,.T.);
#1301=FACE_OUTER_BOUND('',#1971,.T.);
#1302=FACE_OUTER_BOUND('',#1973,.T.);
#1303=FACE_OUTER_BOUND('',#1975,.T.);
#1304=FACE_OUTER_BOUND('',#1977,.T.);
#1305=FACE_OUTER_BOUND('',#1978,.T.);
#1306=FACE_OUTER_BOUND('',#1979,.T.);
#1307=FACE_OUTER_BOUND('',#1980,.T.);
#1308=FACE_OUTER_BOUND('',#1981,.T.);
#1309=FACE_OUTER_BOUND('',#1982,.T.);
#1310=FACE_OUTER_BOUND('',#1984,.T.);
#1311=FACE_OUTER_BOUND('',#1985,.T.);
#1312=FACE_OUTER_BOUND('',#1986,.T.);
#1313=FACE_OUTER_BOUND('',#1987,.T.);
#1314=FACE_OUTER_BOUND('',#1988,.T.);
#1315=FACE_OUTER_BOUND('',#1989,.T.);
#1316=FACE_OUTER_BOUND('',#1990,.T.);
#1317=FACE_OUTER_BOUND('',#1991,.T.);
#1318=FACE_OUTER_BOUND('',#1992,.T.);
#1319=FACE_OUTER_BOUND('',#1993,.T.);
#1320=FACE_OUTER_BOUND('',#1994,.T.);
#1321=FACE_OUTER_BOUND('',#1995,.T.);
#1322=FACE_OUTER_BOUND('',#1997,.T.);
#1323=FACE_OUTER_BOUND('',#1998,.T.);
#1324=FACE_OUTER_BOUND('',#1999,.T.);
#1325=FACE_OUTER_BOUND('',#2000,.T.);
#1326=FACE_OUTER_BOUND('',#2001,.T.);
#1327=FACE_OUTER_BOUND('',#2002,.T.);
#1328=FACE_OUTER_BOUND('',#2003,.T.);
#1329=FACE_OUTER_BOUND('',#2004,.T.);
#1330=FACE_OUTER_BOUND('',#2005,.T.);
#1331=FACE_OUTER_BOUND('',#2006,.T.);
#1332=FACE_OUTER_BOUND('',#2007,.T.);
#1333=FACE_OUTER_BOUND('',#2008,.T.);
#1334=FACE_OUTER_BOUND('',#2009,.T.);
#1335=FACE_OUTER_BOUND('',#2010,.T.);
#1336=FACE_OUTER_BOUND('',#2011,.T.);
#1337=FACE_OUTER_BOUND('',#2012,.T.);
#1338=FACE_OUTER_BOUND('',#2013,.T.);
#1339=FACE_OUTER_BOUND('',#2014,.T.);
#1340=FACE_OUTER_BOUND('',#2015,.T.);
#1341=FACE_OUTER_BOUND('',#2016,.T.);
#1342=FACE_OUTER_BOUND('',#2017,.T.);
#1343=FACE_OUTER_BOUND('',#2018,.T.);
#1344=FACE_OUTER_BOUND('',#2019,.T.);
#1345=FACE_OUTER_BOUND('',#2021,.T.);
#1346=FACE_OUTER_BOUND('',#2023,.T.);
#1347=FACE_OUTER_BOUND('',#2025,.T.);
#1348=FACE_OUTER_BOUND('',#2026,.T.);
#1349=FACE_OUTER_BOUND('',#2028,.T.);
#1350=FACE_OUTER_BOUND('',#2029,.T.);
#1351=FACE_OUTER_BOUND('',#2030,.T.);
#1352=FACE_OUTER_BOUND('',#2031,.T.);
#1353=FACE_OUTER_BOUND('',#2032,.T.);
#1354=FACE_OUTER_BOUND('',#2033,.T.);
#1355=FACE_OUTER_BOUND('',#2034,.T.);
#1356=FACE_OUTER_BOUND('',#2035,.T.);
#1357=FACE_OUTER_BOUND('',#2036,.T.);
#1358=FACE_OUTER_BOUND('',#2037,.T.);
#1359=FACE_OUTER_BOUND('',#2038,.T.);
#1360=FACE_OUTER_BOUND('',#2039,.T.);
#1361=FACE_OUTER_BOUND('',#2040,.T.);
#1362=FACE_OUTER_BOUND('',#2041,.T.);
#1363=FACE_OUTER_BOUND('',#2042,.T.);
#1364=FACE_OUTER_BOUND('',#2043,.T.);
#1365=FACE_OUTER_BOUND('',#2044,.T.);
#1366=FACE_OUTER_BOUND('',#2045,.T.);
#1367=FACE_OUTER_BOUND('',#2046,.T.);
#1368=FACE_OUTER_BOUND('',#2047,.T.);
#1369=FACE_OUTER_BOUND('',#2049,.T.);
#1370=FACE_OUTER_BOUND('',#2051,.T.);
#1371=FACE_OUTER_BOUND('',#2053,.T.);
#1372=FACE_OUTER_BOUND('',#2055,.T.);
#1373=FACE_OUTER_BOUND('',#2056,.T.);
#1374=FACE_OUTER_BOUND('',#2057,.T.);
#1375=FACE_OUTER_BOUND('',#2058,.T.);
#1376=FACE_OUTER_BOUND('',#2059,.T.);
#1377=FACE_OUTER_BOUND('',#2060,.T.);
#1378=FACE_OUTER_BOUND('',#2061,.T.);
#1379=FACE_OUTER_BOUND('',#2062,.T.);
#1380=FACE_OUTER_BOUND('',#2063,.T.);
#1381=FACE_OUTER_BOUND('',#2064,.T.);
#1382=FACE_OUTER_BOUND('',#2065,.T.);
#1383=FACE_OUTER_BOUND('',#2067,.T.);
#1384=FACE_OUTER_BOUND('',#2069,.T.);
#1385=FACE_OUTER_BOUND('',#2071,.T.);
#1386=FACE_OUTER_BOUND('',#2073,.T.);
#1387=FACE_OUTER_BOUND('',#2075,.T.);
#1388=FACE_OUTER_BOUND('',#2077,.T.);
#1389=FACE_OUTER_BOUND('',#2079,.T.);
#1390=FACE_OUTER_BOUND('',#2081,.T.);
#1391=FACE_OUTER_BOUND('',#2082,.T.);
#1392=FACE_OUTER_BOUND('',#2083,.T.);
#1393=FACE_OUTER_BOUND('',#2084,.T.);
#1394=FACE_OUTER_BOUND('',#2085,.T.);
#1395=FACE_OUTER_BOUND('',#2086,.T.);
#1396=FACE_OUTER_BOUND('',#2087,.T.);
#1397=FACE_OUTER_BOUND('',#2088,.T.);
#1398=FACE_OUTER_BOUND('',#2089,.T.);
#1399=FACE_OUTER_BOUND('',#2090,.T.);
#1400=FACE_OUTER_BOUND('',#2091,.T.);
#1401=FACE_OUTER_BOUND('',#2092,.T.);
#1402=FACE_OUTER_BOUND('',#2093,.T.);
#1403=FACE_OUTER_BOUND('',#2094,.T.);
#1404=FACE_OUTER_BOUND('',#2096,.T.);
#1405=FACE_OUTER_BOUND('',#2098,.T.);
#1406=FACE_OUTER_BOUND('',#2100,.T.);
#1407=FACE_OUTER_BOUND('',#2102,.T.);
#1408=FACE_OUTER_BOUND('',#2103,.T.);
#1409=FACE_OUTER_BOUND('',#2104,.T.);
#1410=FACE_OUTER_BOUND('',#2106,.T.);
#1411=FACE_OUTER_BOUND('',#2108,.T.);
#1412=FACE_OUTER_BOUND('',#2109,.T.);
#1413=FACE_OUTER_BOUND('',#2110,.T.);
#1414=FACE_OUTER_BOUND('',#2111,.T.);
#1415=FACE_OUTER_BOUND('',#2112,.T.);
#1416=FACE_OUTER_BOUND('',#2114,.T.);
#1417=EDGE_LOOP('',(#6152,#6153,#6154,#6155));
#1418=EDGE_LOOP('',(#6156,#6157,#6158,#6159));
#1419=EDGE_LOOP('',(#6160,#6161,#6162,#6163));
#1420=EDGE_LOOP('',(#6164,#6165,#6166,#6167));
#1421=EDGE_LOOP('',(#6168,#6169,#6170,#6171));
#1422=EDGE_LOOP('',(#6172,#6173,#6174,#6175));
#1423=EDGE_LOOP('',(#6176,#6177,#6178,#6179));
#1424=EDGE_LOOP('',(#6180,#6181,#6182,#6183));
#1425=EDGE_LOOP('',(#6184,#6185,#6186,#6187));
#1426=EDGE_LOOP('',(#6188,#6189,#6190,#6191));
#1427=EDGE_LOOP('',(#6192,#6193,#6194,#6195));
#1428=EDGE_LOOP('',(#6196,#6197,#6198,#6199));
#1429=EDGE_LOOP('',(#6200,#6201,#6202,#6203));
#1430=EDGE_LOOP('',(#6204,#6205,#6206,#6207));
#1431=EDGE_LOOP('',(#6208,#6209,#6210,#6211));
#1432=EDGE_LOOP('',(#6212,#6213,#6214,#6215));
#1433=EDGE_LOOP('',(#6216,#6217,#6218,#6219));
#1434=EDGE_LOOP('',(#6220,#6221,#6222,#6223));
#1435=EDGE_LOOP('',(#6224,#6225,#6226,#6227));
#1436=EDGE_LOOP('',(#6228,#6229,#6230,#6231));
#1437=EDGE_LOOP('',(#6232,#6233,#6234,#6235));
#1438=EDGE_LOOP('',(#6236,#6237,#6238,#6239));
#1439=EDGE_LOOP('',(#6240,#6241,#6242,#6243));
#1440=EDGE_LOOP('',(#6244,#6245,#6246,#6247));
#1441=EDGE_LOOP('',(#6248,#6249,#6250,#6251));
#1442=EDGE_LOOP('',(#6252,#6253,#6254,#6255));
#1443=EDGE_LOOP('',(#6256,#6257,#6258,#6259));
#1444=EDGE_LOOP('',(#6260,#6261,#6262,#6263));
#1445=EDGE_LOOP('',(#6264,#6265,#6266,#6267));
#1446=EDGE_LOOP('',(#6268,#6269,#6270,#6271));
#1447=EDGE_LOOP('',(#6272,#6273,#6274,#6275));
#1448=EDGE_LOOP('',(#6276,#6277,#6278,#6279));
#1449=EDGE_LOOP('',(#6280,#6281,#6282,#6283));
#1450=EDGE_LOOP('',(#6284,#6285,#6286,#6287));
#1451=EDGE_LOOP('',(#6288,#6289,#6290,#6291));
#1452=EDGE_LOOP('',(#6292,#6293,#6294,#6295));
#1453=EDGE_LOOP('',(#6296));
#1454=EDGE_LOOP('',(#6297));
#1455=EDGE_LOOP('',(#6298));
#1456=EDGE_LOOP('',(#6299));
#1457=EDGE_LOOP('',(#6300,#6301,#6302,#6303));
#1458=EDGE_LOOP('',(#6304,#6305,#6306,#6307));
#1459=EDGE_LOOP('',(#6308));
#1460=EDGE_LOOP('',(#6309));
#1461=EDGE_LOOP('',(#6310));
#1462=EDGE_LOOP('',(#6311));
#1463=EDGE_LOOP('',(#6312,#6313,#6314,#6315));
#1464=EDGE_LOOP('',(#6316,#6317,#6318,#6319));
#1465=EDGE_LOOP('',(#6320,#6321,#6322,#6323,#6324,#6325));
#1466=EDGE_LOOP('',(#6326,#6327,#6328,#6329,#6330,#6331));
#1467=EDGE_LOOP('',(#6332,#6333,#6334,#6335));
#1468=EDGE_LOOP('',(#6336,#6337,#6338,#6339));
#1469=EDGE_LOOP('',(#6340,#6341,#6342,#6343));
#1470=EDGE_LOOP('',(#6344,#6345,#6346,#6347));
#1471=EDGE_LOOP('',(#6348,#6349,#6350,#6351));
#1472=EDGE_LOOP('',(#6352));
#1473=EDGE_LOOP('',(#6353));
#1474=EDGE_LOOP('',(#6354));
#1475=EDGE_LOOP('',(#6355,#6356,#6357,#6358));
#1476=EDGE_LOOP('',(#6359,#6360,#6361,#6362));
#1477=EDGE_LOOP('',(#6363));
#1478=EDGE_LOOP('',(#6364));
#1479=EDGE_LOOP('',(#6365));
#1480=EDGE_LOOP('',(#6366,#6367,#6368,#6369));
#1481=EDGE_LOOP('',(#6370,#6371,#6372,#6373));
#1482=EDGE_LOOP('',(#6374,#6375,#6376,#6377));
#1483=EDGE_LOOP('',(#6378,#6379,#6380,#6381));
#1484=EDGE_LOOP('',(#6382,#6383,#6384,#6385,#6386,#6387,#6388,#6389));
#1485=EDGE_LOOP('',(#6390,#6391,#6392,#6393,#6394,#6395,#6396,#6397));
#1486=EDGE_LOOP('',(#6398,#6399,#6400,#6401));
#1487=EDGE_LOOP('',(#6402,#6403,#6404,#6405));
#1488=EDGE_LOOP('',(#6406,#6407,#6408,#6409));
#1489=EDGE_LOOP('',(#6410,#6411,#6412,#6413));
#1490=EDGE_LOOP('',(#6414,#6415,#6416,#6417));
#1491=EDGE_LOOP('',(#6418,#6419,#6420,#6421));
#1492=EDGE_LOOP('',(#6422,#6423,#6424,#6425,#6426,#6427));
#1493=EDGE_LOOP('',(#6428,#6429,#6430,#6431));
#1494=EDGE_LOOP('',(#6432,#6433,#6434,#6435));
#1495=EDGE_LOOP('',(#6436,#6437,#6438,#6439));
#1496=EDGE_LOOP('',(#6440,#6441,#6442,#6443,#6444,#6445));
#1497=EDGE_LOOP('',(#6446));
#1498=EDGE_LOOP('',(#6447));
#1499=EDGE_LOOP('',(#6448,#6449,#6450,#6451,#6452,#6453));
#1500=EDGE_LOOP('',(#6454));
#1501=EDGE_LOOP('',(#6455));
#1502=EDGE_LOOP('',(#6456,#6457,#6458,#6459));
#1503=EDGE_LOOP('',(#6460,#6461,#6462,#6463));
#1504=EDGE_LOOP('',(#6464,#6465,#6466,#6467));
#1505=EDGE_LOOP('',(#6468,#6469,#6470,#6471));
#1506=EDGE_LOOP('',(#6472,#6473,#6474,#6475));
#1507=EDGE_LOOP('',(#6476,#6477,#6478,#6479,#6480,#6481));
#1508=EDGE_LOOP('',(#6482,#6483,#6484,#6485));
#1509=EDGE_LOOP('',(#6486,#6487,#6488,#6489));
#1510=EDGE_LOOP('',(#6490,#6491,#6492,#6493));
#1511=EDGE_LOOP('',(#6494,#6495,#6496,#6497,#6498,#6499));
#1512=EDGE_LOOP('',(#6500));
#1513=EDGE_LOOP('',(#6501));
#1514=EDGE_LOOP('',(#6502,#6503,#6504,#6505,#6506,#6507));
#1515=EDGE_LOOP('',(#6508));
#1516=EDGE_LOOP('',(#6509));
#1517=EDGE_LOOP('',(#6510,#6511,#6512,#6513));
#1518=EDGE_LOOP('',(#6514,#6515,#6516,#6517));
#1519=EDGE_LOOP('',(#6518,#6519,#6520,#6521));
#1520=EDGE_LOOP('',(#6522,#6523,#6524,#6525));
#1521=EDGE_LOOP('',(#6526,#6527,#6528,#6529));
#1522=EDGE_LOOP('',(#6530,#6531,#6532,#6533));
#1523=EDGE_LOOP('',(#6534,#6535,#6536,#6537));
#1524=EDGE_LOOP('',(#6538,#6539,#6540,#6541));
#1525=EDGE_LOOP('',(#6542,#6543,#6544,#6545));
#1526=EDGE_LOOP('',(#6546,#6547,#6548,#6549));
#1527=EDGE_LOOP('',(#6550,#6551,#6552,#6553));
#1528=EDGE_LOOP('',(#6554,#6555,#6556,#6557));
#1529=EDGE_LOOP('',(#6558,#6559,#6560,#6561));
#1530=EDGE_LOOP('',(#6562,#6563,#6564,#6565));
#1531=EDGE_LOOP('',(#6566,#6567,#6568,#6569));
#1532=EDGE_LOOP('',(#6570,#6571,#6572,#6573));
#1533=EDGE_LOOP('',(#6574,#6575,#6576,#6577));
#1534=EDGE_LOOP('',(#6578,#6579,#6580,#6581));
#1535=EDGE_LOOP('',(#6582,#6583,#6584,#6585));
#1536=EDGE_LOOP('',(#6586,#6587,#6588,#6589));
#1537=EDGE_LOOP('',(#6590,#6591,#6592,#6593));
#1538=EDGE_LOOP('',(#6594,#6595,#6596,#6597));
#1539=EDGE_LOOP('',(#6598,#6599,#6600,#6601));
#1540=EDGE_LOOP('',(#6602,#6603,#6604,#6605));
#1541=EDGE_LOOP('',(#6606,#6607,#6608,#6609));
#1542=EDGE_LOOP('',(#6610,#6611,#6612,#6613));
#1543=EDGE_LOOP('',(#6614,#6615,#6616,#6617));
#1544=EDGE_LOOP('',(#6618,#6619,#6620,#6621));
#1545=EDGE_LOOP('',(#6622,#6623,#6624,#6625));
#1546=EDGE_LOOP('',(#6626,#6627,#6628,#6629));
#1547=EDGE_LOOP('',(#6630,#6631,#6632,#6633));
#1548=EDGE_LOOP('',(#6634,#6635,#6636,#6637));
#1549=EDGE_LOOP('',(#6638,#6639,#6640,#6641));
#1550=EDGE_LOOP('',(#6642,#6643,#6644,#6645));
#1551=EDGE_LOOP('',(#6646,#6647,#6648,#6649));
#1552=EDGE_LOOP('',(#6650,#6651,#6652,#6653));
#1553=EDGE_LOOP('',(#6654));
#1554=EDGE_LOOP('',(#6655));
#1555=EDGE_LOOP('',(#6656,#6657,#6658,#6659));
#1556=EDGE_LOOP('',(#6660,#6661,#6662,#6663));
#1557=EDGE_LOOP('',(#6664));
#1558=EDGE_LOOP('',(#6665));
#1559=EDGE_LOOP('',(#6666,#6667,#6668,#6669));
#1560=EDGE_LOOP('',(#6670,#6671,#6672,#6673));
#1561=EDGE_LOOP('',(#6674,#6675,#6676,#6677));
#1562=EDGE_LOOP('',(#6678,#6679,#6680,#6681));
#1563=EDGE_LOOP('',(#6682,#6683,#6684,#6685,#6686,#6687));
#1564=EDGE_LOOP('',(#6688,#6689,#6690,#6691,#6692,#6693));
#1565=EDGE_LOOP('',(#6694,#6695,#6696,#6697));
#1566=EDGE_LOOP('',(#6698,#6699,#6700,#6701));
#1567=EDGE_LOOP('',(#6702,#6703,#6704,#6705));
#1568=EDGE_LOOP('',(#6706));
#1569=EDGE_LOOP('',(#6707));
#1570=EDGE_LOOP('',(#6708,#6709,#6710,#6711));
#1571=EDGE_LOOP('',(#6712,#6713,#6714,#6715));
#1572=EDGE_LOOP('',(#6716));
#1573=EDGE_LOOP('',(#6717));
#1574=EDGE_LOOP('',(#6718,#6719,#6720,#6721));
#1575=EDGE_LOOP('',(#6722,#6723,#6724,#6725));
#1576=EDGE_LOOP('',(#6726,#6727,#6728,#6729,#6730,#6731,#6732,#6733));
#1577=EDGE_LOOP('',(#6734,#6735,#6736,#6737,#6738,#6739,#6740,#6741));
#1578=EDGE_LOOP('',(#6742,#6743,#6744,#6745));
#1579=EDGE_LOOP('',(#6746,#6747,#6748,#6749));
#1580=EDGE_LOOP('',(#6750,#6751,#6752,#6753));
#1581=EDGE_LOOP('',(#6754,#6755,#6756,#6757));
#1582=EDGE_LOOP('',(#6758,#6759,#6760,#6761));
#1583=EDGE_LOOP('',(#6762,#6763,#6764,#6765));
#1584=EDGE_LOOP('',(#6766,#6767,#6768,#6769));
#1585=EDGE_LOOP('',(#6770,#6771,#6772,#6773));
#1586=EDGE_LOOP('',(#6774,#6775,#6776,#6777,#6778,#6779));
#1587=EDGE_LOOP('',(#6780,#6781,#6782,#6783));
#1588=EDGE_LOOP('',(#6784,#6785,#6786,#6787));
#1589=EDGE_LOOP('',(#6788,#6789,#6790,#6791));
#1590=EDGE_LOOP('',(#6792,#6793,#6794,#6795,#6796,#6797));
#1591=EDGE_LOOP('',(#6798));
#1592=EDGE_LOOP('',(#6799));
#1593=EDGE_LOOP('',(#6800,#6801,#6802,#6803,#6804,#6805));
#1594=EDGE_LOOP('',(#6806));
#1595=EDGE_LOOP('',(#6807));
#1596=EDGE_LOOP('',(#6808,#6809,#6810,#6811));
#1597=EDGE_LOOP('',(#6812,#6813,#6814,#6815));
#1598=EDGE_LOOP('',(#6816,#6817,#6818,#6819));
#1599=EDGE_LOOP('',(#6820,#6821,#6822,#6823));
#1600=EDGE_LOOP('',(#6824,#6825,#6826,#6827));
#1601=EDGE_LOOP('',(#6828,#6829,#6830,#6831,#6832,#6833));
#1602=EDGE_LOOP('',(#6834,#6835,#6836,#6837));
#1603=EDGE_LOOP('',(#6838,#6839,#6840,#6841));
#1604=EDGE_LOOP('',(#6842,#6843,#6844,#6845));
#1605=EDGE_LOOP('',(#6846,#6847,#6848,#6849,#6850,#6851));
#1606=EDGE_LOOP('',(#6852));
#1607=EDGE_LOOP('',(#6853));
#1608=EDGE_LOOP('',(#6854,#6855,#6856,#6857,#6858,#6859));
#1609=EDGE_LOOP('',(#6860));
#1610=EDGE_LOOP('',(#6861));
#1611=EDGE_LOOP('',(#6862,#6863,#6864,#6865));
#1612=EDGE_LOOP('',(#6866,#6867,#6868,#6869));
#1613=EDGE_LOOP('',(#6870,#6871,#6872,#6873));
#1614=EDGE_LOOP('',(#6874,#6875,#6876,#6877));
#1615=EDGE_LOOP('',(#6878,#6879,#6880,#6881));
#1616=EDGE_LOOP('',(#6882,#6883,#6884,#6885));
#1617=EDGE_LOOP('',(#6886,#6887,#6888,#6889));
#1618=EDGE_LOOP('',(#6890,#6891,#6892,#6893));
#1619=EDGE_LOOP('',(#6894,#6895,#6896,#6897));
#1620=EDGE_LOOP('',(#6898,#6899,#6900,#6901));
#1621=EDGE_LOOP('',(#6902,#6903,#6904,#6905));
#1622=EDGE_LOOP('',(#6906,#6907,#6908,#6909));
#1623=EDGE_LOOP('',(#6910,#6911,#6912,#6913));
#1624=EDGE_LOOP('',(#6914,#6915,#6916,#6917));
#1625=EDGE_LOOP('',(#6918,#6919,#6920,#6921));
#1626=EDGE_LOOP('',(#6922,#6923,#6924,#6925));
#1627=EDGE_LOOP('',(#6926,#6927,#6928,#6929));
#1628=EDGE_LOOP('',(#6930,#6931,#6932,#6933));
#1629=EDGE_LOOP('',(#6934,#6935,#6936,#6937));
#1630=EDGE_LOOP('',(#6938,#6939,#6940,#6941));
#1631=EDGE_LOOP('',(#6942,#6943,#6944,#6945));
#1632=EDGE_LOOP('',(#6946,#6947,#6948,#6949));
#1633=EDGE_LOOP('',(#6950,#6951,#6952,#6953));
#1634=EDGE_LOOP('',(#6954,#6955,#6956,#6957));
#1635=EDGE_LOOP('',(#6958,#6959,#6960,#6961,#6962,#6963,#6964,#6965));
#1636=EDGE_LOOP('',(#6966,#6967,#6968,#6969));
#1637=EDGE_LOOP('',(#6970,#6971,#6972,#6973));
#1638=EDGE_LOOP('',(#6974));
#1639=EDGE_LOOP('',(#6975));
#1640=EDGE_LOOP('',(#6976));
#1641=EDGE_LOOP('',(#6977));
#1642=EDGE_LOOP('',(#6978,#6979,#6980,#6981));
#1643=EDGE_LOOP('',(#6982,#6983,#6984,#6985));
#1644=EDGE_LOOP('',(#6986));
#1645=EDGE_LOOP('',(#6987));
#1646=EDGE_LOOP('',(#6988));
#1647=EDGE_LOOP('',(#6989));
#1648=EDGE_LOOP('',(#6990,#6991,#6992,#6993));
#1649=EDGE_LOOP('',(#6994,#6995,#6996,#6997));
#1650=EDGE_LOOP('',(#6998));
#1651=EDGE_LOOP('',(#6999));
#1652=EDGE_LOOP('',(#7000));
#1653=EDGE_LOOP('',(#7001));
#1654=EDGE_LOOP('',(#7002,#7003,#7004,#7005));
#1655=EDGE_LOOP('',(#7006,#7007,#7008,#7009));
#1656=EDGE_LOOP('',(#7010));
#1657=EDGE_LOOP('',(#7011));
#1658=EDGE_LOOP('',(#7012));
#1659=EDGE_LOOP('',(#7013));
#1660=EDGE_LOOP('',(#7014,#7015,#7016,#7017));
#1661=EDGE_LOOP('',(#7018,#7019,#7020,#7021,#7022,#7023,#7024,#7025));
#1662=EDGE_LOOP('',(#7026,#7027,#7028,#7029));
#1663=EDGE_LOOP('',(#7030,#7031,#7032,#7033));
#1664=EDGE_LOOP('',(#7034,#7035,#7036,#7037));
#1665=EDGE_LOOP('',(#7038,#7039,#7040,#7041,#7042,#7043,#7044,#7045));
#1666=EDGE_LOOP('',(#7046,#7047,#7048,#7049,#7050,#7051,#7052,#7053));
#1667=EDGE_LOOP('',(#7054,#7055,#7056,#7057));
#1668=EDGE_LOOP('',(#7058,#7059,#7060,#7061));
#1669=EDGE_LOOP('',(#7062,#7063,#7064,#7065));
#1670=EDGE_LOOP('',(#7066,#7067,#7068,#7069));
#1671=EDGE_LOOP('',(#7070,#7071,#7072,#7073));
#1672=EDGE_LOOP('',(#7074,#7075,#7076,#7077));
#1673=EDGE_LOOP('',(#7078,#7079,#7080,#7081));
#1674=EDGE_LOOP('',(#7082,#7083,#7084,#7085));
#1675=EDGE_LOOP('',(#7086,#7087,#7088,#7089));
#1676=EDGE_LOOP('',(#7090,#7091,#7092,#7093));
#1677=EDGE_LOOP('',(#7094,#7095,#7096,#7097));
#1678=EDGE_LOOP('',(#7098,#7099,#7100,#7101));
#1679=EDGE_LOOP('',(#7102,#7103,#7104,#7105));
#1680=EDGE_LOOP('',(#7106,#7107,#7108,#7109));
#1681=EDGE_LOOP('',(#7110,#7111,#7112,#7113));
#1682=EDGE_LOOP('',(#7114,#7115,#7116,#7117));
#1683=EDGE_LOOP('',(#7118,#7119,#7120,#7121));
#1684=EDGE_LOOP('',(#7122,#7123,#7124,#7125));
#1685=EDGE_LOOP('',(#7126,#7127,#7128,#7129));
#1686=EDGE_LOOP('',(#7130,#7131,#7132,#7133));
#1687=EDGE_LOOP('',(#7134,#7135,#7136,#7137));
#1688=EDGE_LOOP('',(#7138,#7139,#7140,#7141));
#1689=EDGE_LOOP('',(#7142,#7143,#7144,#7145,#7146,#7147,#7148,#7149));
#1690=EDGE_LOOP('',(#7150,#7151,#7152,#7153));
#1691=EDGE_LOOP('',(#7154,#7155,#7156,#7157));
#1692=EDGE_LOOP('',(#7158));
#1693=EDGE_LOOP('',(#7159));
#1694=EDGE_LOOP('',(#7160));
#1695=EDGE_LOOP('',(#7161));
#1696=EDGE_LOOP('',(#7162,#7163,#7164,#7165));
#1697=EDGE_LOOP('',(#7166,#7167,#7168,#7169));
#1698=EDGE_LOOP('',(#7170));
#1699=EDGE_LOOP('',(#7171));
#1700=EDGE_LOOP('',(#7172));
#1701=EDGE_LOOP('',(#7173));
#1702=EDGE_LOOP('',(#7174,#7175,#7176,#7177));
#1703=EDGE_LOOP('',(#7178,#7179,#7180,#7181));
#1704=EDGE_LOOP('',(#7182));
#1705=EDGE_LOOP('',(#7183));
#1706=EDGE_LOOP('',(#7184));
#1707=EDGE_LOOP('',(#7185));
#1708=EDGE_LOOP('',(#7186,#7187,#7188,#7189));
#1709=EDGE_LOOP('',(#7190,#7191,#7192,#7193));
#1710=EDGE_LOOP('',(#7194));
#1711=EDGE_LOOP('',(#7195));
#1712=EDGE_LOOP('',(#7196));
#1713=EDGE_LOOP('',(#7197));
#1714=EDGE_LOOP('',(#7198,#7199,#7200,#7201));
#1715=EDGE_LOOP('',(#7202,#7203,#7204,#7205,#7206,#7207,#7208,#7209));
#1716=EDGE_LOOP('',(#7210,#7211,#7212,#7213));
#1717=EDGE_LOOP('',(#7214,#7215,#7216,#7217));
#1718=EDGE_LOOP('',(#7218,#7219,#7220,#7221));
#1719=EDGE_LOOP('',(#7222,#7223,#7224,#7225,#7226,#7227,#7228,#7229));
#1720=EDGE_LOOP('',(#7230,#7231,#7232,#7233,#7234,#7235,#7236,#7237));
#1721=EDGE_LOOP('',(#7238,#7239,#7240,#7241));
#1722=EDGE_LOOP('',(#7242,#7243,#7244,#7245));
#1723=EDGE_LOOP('',(#7246,#7247,#7248,#7249));
#1724=EDGE_LOOP('',(#7250,#7251,#7252,#7253));
#1725=EDGE_LOOP('',(#7254,#7255,#7256,#7257));
#1726=EDGE_LOOP('',(#7258,#7259,#7260,#7261));
#1727=EDGE_LOOP('',(#7262,#7263,#7264,#7265));
#1728=EDGE_LOOP('',(#7266,#7267,#7268,#7269));
#1729=EDGE_LOOP('',(#7270,#7271,#7272,#7273));
#1730=EDGE_LOOP('',(#7274,#7275,#7276,#7277));
#1731=EDGE_LOOP('',(#7278,#7279,#7280,#7281));
#1732=EDGE_LOOP('',(#7282,#7283,#7284,#7285));
#1733=EDGE_LOOP('',(#7286,#7287,#7288,#7289));
#1734=EDGE_LOOP('',(#7290,#7291,#7292,#7293));
#1735=EDGE_LOOP('',(#7294,#7295,#7296,#7297));
#1736=EDGE_LOOP('',(#7298,#7299,#7300,#7301));
#1737=EDGE_LOOP('',(#7302,#7303,#7304,#7305));
#1738=EDGE_LOOP('',(#7306,#7307,#7308,#7309));
#1739=EDGE_LOOP('',(#7310,#7311,#7312,#7313));
#1740=EDGE_LOOP('',(#7314,#7315,#7316,#7317));
#1741=EDGE_LOOP('',(#7318,#7319,#7320,#7321));
#1742=EDGE_LOOP('',(#7322,#7323,#7324,#7325,#7326,#7327,#7328,#7329));
#1743=EDGE_LOOP('',(#7330,#7331,#7332,#7333));
#1744=EDGE_LOOP('',(#7334,#7335,#7336,#7337));
#1745=EDGE_LOOP('',(#7338,#7339,#7340,#7341));
#1746=EDGE_LOOP('',(#7342,#7343,#7344,#7345));
#1747=EDGE_LOOP('',(#7346,#7347,#7348,#7349));
#1748=EDGE_LOOP('',(#7350,#7351,#7352,#7353));
#1749=EDGE_LOOP('',(#7354));
#1750=EDGE_LOOP('',(#7355));
#1751=EDGE_LOOP('',(#7356));
#1752=EDGE_LOOP('',(#7357,#7358,#7359,#7360));
#1753=EDGE_LOOP('',(#7361,#7362,#7363,#7364));
#1754=EDGE_LOOP('',(#7365));
#1755=EDGE_LOOP('',(#7366));
#1756=EDGE_LOOP('',(#7367));
#1757=EDGE_LOOP('',(#7368,#7369,#7370,#7371));
#1758=EDGE_LOOP('',(#7372,#7373,#7374,#7375));
#1759=EDGE_LOOP('',(#7376,#7377,#7378,#7379));
#1760=EDGE_LOOP('',(#7380,#7381,#7382,#7383));
#1761=EDGE_LOOP('',(#7384,#7385,#7386,#7387));
#1762=EDGE_LOOP('',(#7388,#7389,#7390,#7391,#7392,#7393,#7394,#7395));
#1763=EDGE_LOOP('',(#7396,#7397,#7398,#7399));
#1764=EDGE_LOOP('',(#7400,#7401,#7402,#7403));
#1765=EDGE_LOOP('',(#7404,#7405,#7406,#7407,#7408,#7409,#7410,#7411));
#1766=EDGE_LOOP('',(#7412,#7413,#7414,#7415));
#1767=EDGE_LOOP('',(#7416,#7417,#7418,#7419,#7420,#7421,#7422,#7423));
#1768=EDGE_LOOP('',(#7424,#7425,#7426,#7427));
#1769=EDGE_LOOP('',(#7428,#7429,#7430,#7431));
#1770=EDGE_LOOP('',(#7432,#7433,#7434,#7435));
#1771=EDGE_LOOP('',(#7436,#7437,#7438,#7439));
#1772=EDGE_LOOP('',(#7440,#7441,#7442,#7443));
#1773=EDGE_LOOP('',(#7444,#7445,#7446,#7447));
#1774=EDGE_LOOP('',(#7448,#7449,#7450,#7451));
#1775=EDGE_LOOP('',(#7452,#7453,#7454,#7455));
#1776=EDGE_LOOP('',(#7456,#7457,#7458,#7459));
#1777=EDGE_LOOP('',(#7460,#7461,#7462,#7463));
#1778=EDGE_LOOP('',(#7464,#7465,#7466,#7467));
#1779=EDGE_LOOP('',(#7468,#7469,#7470,#7471));
#1780=EDGE_LOOP('',(#7472,#7473,#7474,#7475));
#1781=EDGE_LOOP('',(#7476,#7477,#7478,#7479));
#1782=EDGE_LOOP('',(#7480,#7481,#7482,#7483));
#1783=EDGE_LOOP('',(#7484,#7485,#7486,#7487));
#1784=EDGE_LOOP('',(#7488,#7489,#7490,#7491));
#1785=EDGE_LOOP('',(#7492,#7493,#7494,#7495));
#1786=EDGE_LOOP('',(#7496,#7497,#7498,#7499));
#1787=EDGE_LOOP('',(#7500,#7501,#7502,#7503));
#1788=EDGE_LOOP('',(#7504,#7505,#7506,#7507));
#1789=EDGE_LOOP('',(#7508,#7509,#7510,#7511));
#1790=EDGE_LOOP('',(#7512,#7513,#7514,#7515));
#1791=EDGE_LOOP('',(#7516,#7517,#7518,#7519));
#1792=EDGE_LOOP('',(#7520,#7521,#7522,#7523));
#1793=EDGE_LOOP('',(#7524,#7525,#7526,#7527,#7528,#7529,#7530,#7531,#7532,
#7533,#7534,#7535,#7536,#7537));
#1794=EDGE_LOOP('',(#7538,#7539,#7540,#7541,#7542,#7543,#7544,#7545));
#1795=EDGE_LOOP('',(#7546,#7547,#7548,#7549));
#1796=EDGE_LOOP('',(#7550,#7551,#7552,#7553,#7554,#7555,#7556,#7557,#7558,
#7559,#7560,#7561,#7562,#7563,#7564,#7565,#7566,#7567,#7568,#7569));
#1797=EDGE_LOOP('',(#7570,#7571,#7572,#7573,#7574,#7575,#7576,#7577));
#1798=EDGE_LOOP('',(#7578,#7579,#7580,#7581,#7582,#7583,#7584,#7585,#7586,
#7587,#7588,#7589,#7590,#7591,#7592,#7593,#7594,#7595,#7596,#7597,#7598,
#7599,#7600,#7601,#7602,#7603,#7604,#7605));
#1799=EDGE_LOOP('',(#7606,#7607,#7608,#7609));
#1800=EDGE_LOOP('',(#7610,#7611,#7612,#7613));
#1801=EDGE_LOOP('',(#7614,#7615,#7616,#7617));
#1802=EDGE_LOOP('',(#7618,#7619,#7620,#7621));
#1803=EDGE_LOOP('',(#7622,#7623,#7624,#7625));
#1804=EDGE_LOOP('',(#7626,#7627,#7628,#7629));
#1805=EDGE_LOOP('',(#7630,#7631,#7632,#7633));
#1806=EDGE_LOOP('',(#7634,#7635,#7636,#7637));
#1807=EDGE_LOOP('',(#7638,#7639,#7640,#7641));
#1808=EDGE_LOOP('',(#7642,#7643,#7644,#7645));
#1809=EDGE_LOOP('',(#7646,#7647,#7648,#7649));
#1810=EDGE_LOOP('',(#7650,#7651,#7652,#7653));
#1811=EDGE_LOOP('',(#7654,#7655,#7656,#7657));
#1812=EDGE_LOOP('',(#7658,#7659,#7660,#7661));
#1813=EDGE_LOOP('',(#7662,#7663,#7664,#7665));
#1814=EDGE_LOOP('',(#7666,#7667,#7668,#7669,#7670,#7671,#7672,#7673));
#1815=EDGE_LOOP('',(#7674,#7675,#7676,#7677,#7678,#7679,#7680,#7681,#7682,
#7683,#7684,#7685));
#1816=EDGE_LOOP('',(#7686,#7687,#7688,#7689));
#1817=EDGE_LOOP('',(#7690,#7691,#7692,#7693));
#1818=EDGE_LOOP('',(#7694,#7695,#7696,#7697));
#1819=EDGE_LOOP('',(#7698));
#1820=EDGE_LOOP('',(#7699,#7700,#7701,#7702));
#1821=EDGE_LOOP('',(#7703,#7704,#7705,#7706));
#1822=EDGE_LOOP('',(#7707,#7708,#7709,#7710));
#1823=EDGE_LOOP('',(#7711,#7712,#7713,#7714));
#1824=EDGE_LOOP('',(#7715,#7716,#7717,#7718,#7719));
#1825=EDGE_LOOP('',(#7720));
#1826=EDGE_LOOP('',(#7721,#7722,#7723,#7724,#7725));
#1827=EDGE_LOOP('',(#7726));
#1828=EDGE_LOOP('',(#7727,#7728,#7729,#7730));
#1829=EDGE_LOOP('',(#7731));
#1830=EDGE_LOOP('',(#7732,#7733,#7734,#7735));
#1831=EDGE_LOOP('',(#7736,#7737,#7738,#7739));
#1832=EDGE_LOOP('',(#7740,#7741,#7742,#7743));
#1833=EDGE_LOOP('',(#7744,#7745,#7746,#7747));
#1834=EDGE_LOOP('',(#7748,#7749,#7750,#7751));
#1835=EDGE_LOOP('',(#7752,#7753,#7754,#7755));
#1836=EDGE_LOOP('',(#7756,#7757,#7758,#7759));
#1837=EDGE_LOOP('',(#7760,#7761,#7762,#7763));
#1838=EDGE_LOOP('',(#7764,#7765,#7766,#7767));
#1839=EDGE_LOOP('',(#7768,#7769,#7770,#7771));
#1840=EDGE_LOOP('',(#7772,#7773,#7774,#7775));
#1841=EDGE_LOOP('',(#7776,#7777,#7778,#7779));
#1842=EDGE_LOOP('',(#7780,#7781,#7782,#7783));
#1843=EDGE_LOOP('',(#7784,#7785,#7786,#7787));
#1844=EDGE_LOOP('',(#7788,#7789,#7790,#7791));
#1845=EDGE_LOOP('',(#7792,#7793,#7794,#7795));
#1846=EDGE_LOOP('',(#7796,#7797,#7798,#7799));
#1847=EDGE_LOOP('',(#7800,#7801,#7802,#7803));
#1848=EDGE_LOOP('',(#7804,#7805,#7806,#7807));
#1849=EDGE_LOOP('',(#7808,#7809,#7810,#7811));
#1850=EDGE_LOOP('',(#7812,#7813,#7814,#7815));
#1851=EDGE_LOOP('',(#7816,#7817,#7818,#7819));
#1852=EDGE_LOOP('',(#7820,#7821,#7822,#7823));
#1853=EDGE_LOOP('',(#7824,#7825,#7826,#7827));
#1854=EDGE_LOOP('',(#7828,#7829,#7830,#7831,#7832,#7833,#7834,#7835,#7836,
#7837,#7838,#7839,#7840,#7841,#7842,#7843,#7844,#7845,#7846,#7847,#7848,
#7849,#7850,#7851,#7852,#7853,#7854,#7855));
#1855=EDGE_LOOP('',(#7856,#7857,#7858,#7859));
#1856=EDGE_LOOP('',(#7860,#7861,#7862,#7863));
#1857=EDGE_LOOP('',(#7864,#7865,#7866,#7867));
#1858=EDGE_LOOP('',(#7868,#7869,#7870,#7871));
#1859=EDGE_LOOP('',(#7872,#7873,#7874,#7875));
#1860=EDGE_LOOP('',(#7876,#7877,#7878,#7879));
#1861=EDGE_LOOP('',(#7880,#7881,#7882,#7883));
#1862=EDGE_LOOP('',(#7884,#7885,#7886,#7887,#7888,#7889,#7890,#7891));
#1863=EDGE_LOOP('',(#7892,#7893,#7894,#7895,#7896,#7897,#7898,#7899));
#1864=EDGE_LOOP('',(#7900,#7901,#7902,#7903));
#1865=EDGE_LOOP('',(#7904,#7905,#7906,#7907));
#1866=EDGE_LOOP('',(#7908,#7909,#7910,#7911));
#1867=EDGE_LOOP('',(#7912,#7913,#7914,#7915));
#1868=EDGE_LOOP('',(#7916,#7917,#7918,#7919));
#1869=EDGE_LOOP('',(#7920,#7921,#7922,#7923));
#1870=EDGE_LOOP('',(#7924,#7925,#7926,#7927));
#1871=EDGE_LOOP('',(#7928,#7929,#7930,#7931,#7932,#7933,#7934,#7935));
#1872=EDGE_LOOP('',(#7936,#7937,#7938,#7939));
#1873=EDGE_LOOP('',(#7940,#7941,#7942,#7943));
#1874=EDGE_LOOP('',(#7944,#7945,#7946,#7947));
#1875=EDGE_LOOP('',(#7948,#7949,#7950,#7951));
#1876=EDGE_LOOP('',(#7952,#7953,#7954,#7955));
#1877=EDGE_LOOP('',(#7956,#7957,#7958,#7959));
#1878=EDGE_LOOP('',(#7960,#7961,#7962,#7963));
#1879=EDGE_LOOP('',(#7964,#7965,#7966,#7967));
#1880=EDGE_LOOP('',(#7968,#7969,#7970,#7971));
#1881=EDGE_LOOP('',(#7972,#7973,#7974,#7975));
#1882=EDGE_LOOP('',(#7976,#7977,#7978,#7979));
#1883=EDGE_LOOP('',(#7980,#7981,#7982,#7983));
#1884=EDGE_LOOP('',(#7984,#7985,#7986,#7987));
#1885=EDGE_LOOP('',(#7988,#7989,#7990,#7991));
#1886=EDGE_LOOP('',(#7992,#7993,#7994,#7995));
#1887=EDGE_LOOP('',(#7996,#7997,#7998,#7999));
#1888=EDGE_LOOP('',(#8000,#8001,#8002,#8003));
#1889=EDGE_LOOP('',(#8004,#8005,#8006,#8007));
#1890=EDGE_LOOP('',(#8008,#8009,#8010,#8011,#8012,#8013,#8014,#8015,#8016,
#8017,#8018,#8019,#8020,#8021,#8022,#8023,#8024,#8025,#8026,#8027));
#1891=EDGE_LOOP('',(#8028,#8029,#8030,#8031));
#1892=EDGE_LOOP('',(#8032,#8033,#8034,#8035));
#1893=EDGE_LOOP('',(#8036,#8037,#8038,#8039));
#1894=EDGE_LOOP('',(#8040,#8041,#8042,#8043));
#1895=EDGE_LOOP('',(#8044,#8045,#8046,#8047));
#1896=EDGE_LOOP('',(#8048,#8049,#8050,#8051));
#1897=EDGE_LOOP('',(#8052,#8053,#8054,#8055));
#1898=EDGE_LOOP('',(#8056,#8057,#8058,#8059));
#1899=EDGE_LOOP('',(#8060,#8061,#8062,#8063));
#1900=EDGE_LOOP('',(#8064,#8065,#8066,#8067));
#1901=EDGE_LOOP('',(#8068,#8069,#8070,#8071));
#1902=EDGE_LOOP('',(#8072,#8073,#8074,#8075));
#1903=EDGE_LOOP('',(#8076,#8077,#8078,#8079));
#1904=EDGE_LOOP('',(#8080,#8081,#8082,#8083));
#1905=EDGE_LOOP('',(#8084,#8085,#8086,#8087,#8088,#8089,#8090,#8091,#8092,
#8093,#8094,#8095,#8096,#8097));
#1906=EDGE_LOOP('',(#8098,#8099,#8100,#8101));
#1907=EDGE_LOOP('',(#8102,#8103,#8104,#8105));
#1908=EDGE_LOOP('',(#8106,#8107,#8108,#8109));
#1909=EDGE_LOOP('',(#8110,#8111,#8112,#8113));
#1910=EDGE_LOOP('',(#8114,#8115,#8116,#8117));
#1911=EDGE_LOOP('',(#8118,#8119,#8120,#8121));
#1912=EDGE_LOOP('',(#8122,#8123,#8124,#8125));
#1913=EDGE_LOOP('',(#8126,#8127,#8128,#8129));
#1914=EDGE_LOOP('',(#8130,#8131,#8132,#8133));
#1915=EDGE_LOOP('',(#8134,#8135,#8136,#8137));
#1916=EDGE_LOOP('',(#8138,#8139,#8140,#8141));
#1917=EDGE_LOOP('',(#8142,#8143,#8144,#8145));
#1918=EDGE_LOOP('',(#8146,#8147,#8148,#8149,#8150,#8151,#8152,#8153));
#1919=EDGE_LOOP('',(#8154,#8155,#8156,#8157,#8158,#8159,#8160,#8161));
#1920=EDGE_LOOP('',(#8162,#8163,#8164,#8165,#8166,#8167,#8168,#8169));
#1921=EDGE_LOOP('',(#8170,#8171,#8172,#8173));
#1922=EDGE_LOOP('',(#8174,#8175,#8176,#8177));
#1923=EDGE_LOOP('',(#8178,#8179,#8180,#8181));
#1924=EDGE_LOOP('',(#8182,#8183,#8184,#8185));
#1925=EDGE_LOOP('',(#8186,#8187,#8188,#8189));
#1926=EDGE_LOOP('',(#8190,#8191,#8192,#8193));
#1927=EDGE_LOOP('',(#8194,#8195,#8196,#8197));
#1928=EDGE_LOOP('',(#8198,#8199,#8200,#8201,#8202));
#1929=EDGE_LOOP('',(#8203));
#1930=EDGE_LOOP('',(#8204,#8205,#8206,#8207,#8208));
#1931=EDGE_LOOP('',(#8209));
#1932=EDGE_LOOP('',(#8210,#8211,#8212,#8213));
#1933=EDGE_LOOP('',(#8214,#8215,#8216,#8217));
#1934=EDGE_LOOP('',(#8218,#8219,#8220,#8221));
#1935=EDGE_LOOP('',(#8222,#8223,#8224,#8225,#8226));
#1936=EDGE_LOOP('',(#8227,#8228,#8229,#8230,#8231));
#1937=EDGE_LOOP('',(#8232,#8233,#8234));
#1938=EDGE_LOOP('',(#8235,#8236,#8237,#8238,#8239,#8240));
#1939=EDGE_LOOP('',(#8241,#8242,#8243));
#1940=EDGE_LOOP('',(#8244,#8245,#8246));
#1941=EDGE_LOOP('',(#8247,#8248,#8249));
#1942=EDGE_LOOP('',(#8250,#8251,#8252));
#1943=EDGE_LOOP('',(#8253,#8254,#8255));
#1944=EDGE_LOOP('',(#8256,#8257,#8258,#8259,#8260));
#1945=EDGE_LOOP('',(#8261,#8262,#8263,#8264,#8265));
#1946=EDGE_LOOP('',(#8266,#8267,#8268,#8269,#8270));
#1947=EDGE_LOOP('',(#8271,#8272,#8273,#8274,#8275));
#1948=EDGE_LOOP('',(#8276,#8277,#8278,#8279,#8280));
#1949=EDGE_LOOP('',(#8281,#8282,#8283,#8284,#8285));
#1950=EDGE_LOOP('',(#8286));
#1951=EDGE_LOOP('',(#8287));
#1952=EDGE_LOOP('',(#8288));
#1953=EDGE_LOOP('',(#8289,#8290,#8291,#8292,#8293,#8294));
#1954=EDGE_LOOP('',(#8295));
#1955=EDGE_LOOP('',(#8296,#8297,#8298,#8299));
#1956=EDGE_LOOP('',(#8300,#8301,#8302,#8303,#8304));
#1957=EDGE_LOOP('',(#8305,#8306,#8307,#8308,#8309,#8310));
#1958=EDGE_LOOP('',(#8311,#8312,#8313,#8314));
#1959=EDGE_LOOP('',(#8315,#8316,#8317,#8318));
#1960=EDGE_LOOP('',(#8319,#8320,#8321,#8322));
#1961=EDGE_LOOP('',(#8323,#8324,#8325,#8326));
#1962=EDGE_LOOP('',(#8327,#8328,#8329,#8330));
#1963=EDGE_LOOP('',(#8331,#8332,#8333,#8334,#8335));
#1964=EDGE_LOOP('',(#8336,#8337,#8338,#8339,#8340,#8341));
#1965=EDGE_LOOP('',(#8342,#8343,#8344,#8345,#8346));
#1966=EDGE_LOOP('',(#8347,#8348,#8349,#8350,#8351));
#1967=EDGE_LOOP('',(#8352));
#1968=EDGE_LOOP('',(#8353));
#1969=EDGE_LOOP('',(#8354));
#1970=EDGE_LOOP('',(#8355));
#1971=EDGE_LOOP('',(#8356));
#1972=EDGE_LOOP('',(#8357));
#1973=EDGE_LOOP('',(#8358));
#1974=EDGE_LOOP('',(#8359));
#1975=EDGE_LOOP('',(#8360));
#1976=EDGE_LOOP('',(#8361));
#1977=EDGE_LOOP('',(#8362,#8363,#8364,#8365,#8366,#8367,#8368,#8369,#8370));
#1978=EDGE_LOOP('',(#8371,#8372,#8373,#8374,#8375));
#1979=EDGE_LOOP('',(#8376,#8377,#8378,#8379,#8380));
#1980=EDGE_LOOP('',(#8381,#8382,#8383,#8384));
#1981=EDGE_LOOP('',(#8385,#8386,#8387));
#1982=EDGE_LOOP('',(#8388,#8389,#8390,#8391,#8392,#8393));
#1983=EDGE_LOOP('',(#8394));
#1984=EDGE_LOOP('',(#8395,#8396,#8397));
#1985=EDGE_LOOP('',(#8398,#8399,#8400));
#1986=EDGE_LOOP('',(#8401,#8402,#8403));
#1987=EDGE_LOOP('',(#8404,#8405,#8406));
#1988=EDGE_LOOP('',(#8407,#8408,#8409));
#1989=EDGE_LOOP('',(#8410,#8411,#8412,#8413,#8414,#8415));
#1990=EDGE_LOOP('',(#8416,#8417,#8418,#8419,#8420,#8421));
#1991=EDGE_LOOP('',(#8422,#8423,#8424,#8425,#8426,#8427));
#1992=EDGE_LOOP('',(#8428,#8429,#8430,#8431,#8432,#8433));
#1993=EDGE_LOOP('',(#8434,#8435,#8436,#8437,#8438,#8439));
#1994=EDGE_LOOP('',(#8440,#8441,#8442,#8443,#8444,#8445));
#1995=EDGE_LOOP('',(#8446));
#1996=EDGE_LOOP('',(#8447));
#1997=EDGE_LOOP('',(#8448,#8449,#8450));
#1998=EDGE_LOOP('',(#8451,#8452,#8453));
#1999=EDGE_LOOP('',(#8454,#8455,#8456));
#2000=EDGE_LOOP('',(#8457,#8458,#8459));
#2001=EDGE_LOOP('',(#8460,#8461,#8462));
#2002=EDGE_LOOP('',(#8463,#8464,#8465));
#2003=EDGE_LOOP('',(#8466,#8467,#8468,#8469,#8470));
#2004=EDGE_LOOP('',(#8471,#8472,#8473,#8474,#8475,#8476,#8477,#8478));
#2005=EDGE_LOOP('',(#8479,#8480,#8481,#8482));
#2006=EDGE_LOOP('',(#8483,#8484,#8485,#8486));
#2007=EDGE_LOOP('',(#8487,#8488,#8489,#8490));
#2008=EDGE_LOOP('',(#8491,#8492,#8493,#8494));
#2009=EDGE_LOOP('',(#8495,#8496,#8497,#8498));
#2010=EDGE_LOOP('',(#8499,#8500,#8501,#8502));
#2011=EDGE_LOOP('',(#8503,#8504,#8505,#8506,#8507));
#2012=EDGE_LOOP('',(#8508,#8509,#8510,#8511,#8512));
#2013=EDGE_LOOP('',(#8513,#8514,#8515,#8516));
#2014=EDGE_LOOP('',(#8517,#8518,#8519,#8520));
#2015=EDGE_LOOP('',(#8521,#8522,#8523,#8524));
#2016=EDGE_LOOP('',(#8525,#8526,#8527));
#2017=EDGE_LOOP('',(#8528,#8529,#8530));
#2018=EDGE_LOOP('',(#8531));
#2019=EDGE_LOOP('',(#8532));
#2020=EDGE_LOOP('',(#8533));
#2021=EDGE_LOOP('',(#8534));
#2022=EDGE_LOOP('',(#8535));
#2023=EDGE_LOOP('',(#8536));
#2024=EDGE_LOOP('',(#8537));
#2025=EDGE_LOOP('',(#8538));
#2026=EDGE_LOOP('',(#8539,#8540,#8541,#8542));
#2027=EDGE_LOOP('',(#8543));
#2028=EDGE_LOOP('',(#8544,#8545,#8546,#8547));
#2029=EDGE_LOOP('',(#8548,#8549,#8550,#8551,#8552));
#2030=EDGE_LOOP('',(#8553,#8554,#8555,#8556));
#2031=EDGE_LOOP('',(#8557,#8558,#8559,#8560,#8561));
#2032=EDGE_LOOP('',(#8562,#8563,#8564,#8565,#8566,#8567));
#2033=EDGE_LOOP('',(#8568,#8569,#8570,#8571));
#2034=EDGE_LOOP('',(#8572,#8573,#8574,#8575));
#2035=EDGE_LOOP('',(#8576,#8577,#8578,#8579));
#2036=EDGE_LOOP('',(#8580,#8581,#8582,#8583,#8584));
#2037=EDGE_LOOP('',(#8585,#8586,#8587,#8588,#8589,#8590));
#2038=EDGE_LOOP('',(#8591,#8592,#8593,#8594,#8595));
#2039=EDGE_LOOP('',(#8596,#8597,#8598,#8599));
#2040=EDGE_LOOP('',(#8600,#8601,#8602,#8603));
#2041=EDGE_LOOP('',(#8604,#8605,#8606,#8607));
#2042=EDGE_LOOP('',(#8608,#8609,#8610,#8611));
#2043=EDGE_LOOP('',(#8612,#8613,#8614,#8615));
#2044=EDGE_LOOP('',(#8616,#8617,#8618,#8619));
#2045=EDGE_LOOP('',(#8620,#8621,#8622,#8623));
#2046=EDGE_LOOP('',(#8624,#8625,#8626,#8627));
#2047=EDGE_LOOP('',(#8628,#8629,#8630,#8631,#8632,#8633,#8634,#8635));
#2048=EDGE_LOOP('',(#8636));
#2049=EDGE_LOOP('',(#8637,#8638,#8639,#8640,#8641,#8642,#8643,#8644));
#2050=EDGE_LOOP('',(#8645));
#2051=EDGE_LOOP('',(#8646));
#2052=EDGE_LOOP('',(#8647));
#2053=EDGE_LOOP('',(#8648));
#2054=EDGE_LOOP('',(#8649));
#2055=EDGE_LOOP('',(#8650,#8651,#8652,#8653));
#2056=EDGE_LOOP('',(#8654,#8655,#8656,#8657));
#2057=EDGE_LOOP('',(#8658,#8659,#8660,#8661));
#2058=EDGE_LOOP('',(#8662,#8663,#8664,#8665));
#2059=EDGE_LOOP('',(#8666,#8667,#8668,#8669));
#2060=EDGE_LOOP('',(#8670,#8671,#8672,#8673));
#2061=EDGE_LOOP('',(#8674,#8675,#8676,#8677));
#2062=EDGE_LOOP('',(#8678,#8679,#8680,#8681));
#2063=EDGE_LOOP('',(#8682,#8683,#8684,#8685));
#2064=EDGE_LOOP('',(#8686,#8687,#8688,#8689));
#2065=EDGE_LOOP('',(#8690));
#2066=EDGE_LOOP('',(#8691));
#2067=EDGE_LOOP('',(#8692));
#2068=EDGE_LOOP('',(#8693));
#2069=EDGE_LOOP('',(#8694));
#2070=EDGE_LOOP('',(#8695));
#2071=EDGE_LOOP('',(#8696));
#2072=EDGE_LOOP('',(#8697));
#2073=EDGE_LOOP('',(#8698));
#2074=EDGE_LOOP('',(#8699));
#2075=EDGE_LOOP('',(#8700));
#2076=EDGE_LOOP('',(#8701));
#2077=EDGE_LOOP('',(#8702));
#2078=EDGE_LOOP('',(#8703));
#2079=EDGE_LOOP('',(#8704));
#2080=EDGE_LOOP('',(#8705));
#2081=EDGE_LOOP('',(#8706,#8707,#8708,#8709));
#2082=EDGE_LOOP('',(#8710,#8711,#8712,#8713));
#2083=EDGE_LOOP('',(#8714,#8715,#8716,#8717));
#2084=EDGE_LOOP('',(#8718,#8719,#8720,#8721));
#2085=EDGE_LOOP('',(#8722,#8723,#8724,#8725));
#2086=EDGE_LOOP('',(#8726,#8727,#8728,#8729,#8730));
#2087=EDGE_LOOP('',(#8731,#8732,#8733,#8734,#8735,#8736));
#2088=EDGE_LOOP('',(#8737,#8738,#8739,#8740,#8741,#8742));
#2089=EDGE_LOOP('',(#8743,#8744,#8745,#8746,#8747,#8748));
#2090=EDGE_LOOP('',(#8749,#8750,#8751,#8752,#8753));
#2091=EDGE_LOOP('',(#8754,#8755,#8756,#8757));
#2092=EDGE_LOOP('',(#8758,#8759,#8760,#8761));
#2093=EDGE_LOOP('',(#8762,#8763,#8764,#8765));
#2094=EDGE_LOOP('',(#8766));
#2095=EDGE_LOOP('',(#8767));
#2096=EDGE_LOOP('',(#8768));
#2097=EDGE_LOOP('',(#8769));
#2098=EDGE_LOOP('',(#8770));
#2099=EDGE_LOOP('',(#8771));
#2100=EDGE_LOOP('',(#8772));
#2101=EDGE_LOOP('',(#8773));
#2102=EDGE_LOOP('',(#8774,#8775,#8776,#8777));
#2103=EDGE_LOOP('',(#8778,#8779,#8780,#8781));
#2104=EDGE_LOOP('',(#8782));
#2105=EDGE_LOOP('',(#8783));
#2106=EDGE_LOOP('',(#8784));
#2107=EDGE_LOOP('',(#8785));
#2108=EDGE_LOOP('',(#8786,#8787,#8788,#8789,#8790));
#2109=EDGE_LOOP('',(#8791,#8792,#8793,#8794,#8795));
#2110=EDGE_LOOP('',(#8796,#8797,#8798,#8799));
#2111=EDGE_LOOP('',(#8800,#8801,#8802,#8803));
#2112=EDGE_LOOP('',(#8804));
#2113=EDGE_LOOP('',(#8805));
#2114=EDGE_LOOP('',(#8806));
#2115=EDGE_LOOP('',(#8807));
#2116=LINE('',#13815,#2840);
#2117=LINE('',#13821,#2841);
#2118=LINE('',#13827,#2842);
#2119=LINE('',#13833,#2843);
#2120=LINE('',#13839,#2844);
#2121=LINE('',#13845,#2845);
#2122=LINE('',#13851,#2846);
#2123=LINE('',#13857,#2847);
#2124=LINE('',#13863,#2848);
#2125=LINE('',#13869,#2849);
#2126=LINE('',#13875,#2850);
#2127=LINE('',#13880,#2851);
#2128=LINE('',#13884,#2852);
#2129=LINE('',#13885,#2853);
#2130=LINE('',#13889,#2854);
#2131=LINE('',#13893,#2855);
#2132=LINE('',#13894,#2856);
#2133=LINE('',#13897,#2857);
#2134=LINE('',#13898,#2858);
#2135=LINE('',#13900,#2859);
#2136=LINE('',#13901,#2860);
#2137=LINE('',#13905,#2861);
#2138=LINE('',#13907,#2862);
#2139=LINE('',#13909,#2863);
#2140=LINE('',#13910,#2864);
#2141=LINE('',#13914,#2865);
#2142=LINE('',#13917,#2866);
#2143=LINE('',#13918,#2867);
#2144=LINE('',#13921,#2868);
#2145=LINE('',#13925,#2869);
#2146=LINE('',#13926,#2870);
#2147=LINE('',#13930,#2871);
#2148=LINE('',#13934,#2872);
#2149=LINE('',#13938,#2873);
#2150=LINE('',#13940,#2874);
#2151=LINE('',#13941,#2875);
#2152=LINE('',#13945,#2876);
#2153=LINE('',#13949,#2877);
#2154=LINE('',#13953,#2878);
#2155=LINE('',#13955,#2879);
#2156=LINE('',#13956,#2880);
#2157=LINE('',#13960,#2881);
#2158=LINE('',#13965,#2882);
#2159=LINE('',#13967,#2883);
#2160=LINE('',#13968,#2884);
#2161=LINE('',#13972,#2885);
#2162=LINE('',#13976,#2886);
#2163=LINE('',#13979,#2887);
#2164=LINE('',#13980,#2888);
#2165=LINE('',#13987,#2889);
#2166=LINE('',#13991,#2890);
#2167=LINE('',#13992,#2891);
#2168=LINE('',#13996,#2892);
#2169=LINE('',#14001,#2893);
#2170=LINE('',#14003,#2894);
#2171=LINE('',#14004,#2895);
#2172=LINE('',#14009,#2896);
#2173=LINE('',#14014,#2897);
#2174=LINE('',#14019,#2898);
#2175=LINE('',#14021,#2899);
#2176=LINE('',#14022,#2900);
#2177=LINE('',#14026,#2901);
#2178=LINE('',#14030,#2902);
#2179=LINE('',#14033,#2903);
#2180=LINE('',#14034,#2904);
#2181=LINE('',#14037,#2905);
#2182=LINE('',#14038,#2906);
#2183=LINE('',#14039,#2907);
#2184=LINE('',#14042,#2908);
#2185=LINE('',#14043,#2909);
#2186=LINE('',#14045,#2910);
#2187=LINE('',#14046,#2911);
#2188=LINE('',#14048,#2912);
#2189=LINE('',#14050,#2913);
#2190=LINE('',#14053,#2914);
#2191=LINE('',#14055,#2915);
#2192=LINE('',#14057,#2916);
#2193=LINE('',#14059,#2917);
#2194=LINE('',#14061,#2918);
#2195=LINE('',#14064,#2919);
#2196=LINE('',#14065,#2920);
#2197=LINE('',#14068,#2921);
#2198=LINE('',#14069,#2922);
#2199=LINE('',#14071,#2923);
#2200=LINE('',#14072,#2924);
#2201=LINE('',#14074,#2925);
#2202=LINE('',#14076,#2926);
#2203=LINE('',#14078,#2927);
#2204=LINE('',#14080,#2928);
#2205=LINE('',#14082,#2929);
#2206=LINE('',#14083,#2930);
#2207=LINE('',#14085,#2931);
#2208=LINE('',#14086,#2932);
#2209=LINE('',#14087,#2933);
#2210=LINE('',#14089,#2934);
#2211=LINE('',#14097,#2935);
#2212=LINE('',#14104,#2936);
#2213=LINE('',#14106,#2937);
#2214=LINE('',#14108,#2938);
#2215=LINE('',#14111,#2939);
#2216=LINE('',#14113,#2940);
#2217=LINE('',#14114,#2941);
#2218=LINE('',#14117,#2942);
#2219=LINE('',#14119,#2943);
#2220=LINE('',#14120,#2944);
#2221=LINE('',#14123,#2945);
#2222=LINE('',#14125,#2946);
#2223=LINE('',#14126,#2947);
#2224=LINE('',#14129,#2948);
#2225=LINE('',#14131,#2949);
#2226=LINE('',#14132,#2950);
#2227=LINE('',#14134,#2951);
#2228=LINE('',#14136,#2952);
#2229=LINE('',#14143,#2953);
#2230=LINE('',#14149,#2954);
#2231=LINE('',#14151,#2955);
#2232=LINE('',#14153,#2956);
#2233=LINE('',#14156,#2957);
#2234=LINE('',#14158,#2958);
#2235=LINE('',#14159,#2959);
#2236=LINE('',#14162,#2960);
#2237=LINE('',#14164,#2961);
#2238=LINE('',#14165,#2962);
#2239=LINE('',#14168,#2963);
#2240=LINE('',#14170,#2964);
#2241=LINE('',#14171,#2965);
#2242=LINE('',#14174,#2966);
#2243=LINE('',#14176,#2967);
#2244=LINE('',#14177,#2968);
#2245=LINE('',#14179,#2969);
#2246=LINE('',#14181,#2970);
#2247=LINE('',#14188,#2971);
#2248=LINE('',#14194,#2972);
#2249=LINE('',#14200,#2973);
#2250=LINE('',#14206,#2974);
#2251=LINE('',#14212,#2975);
#2252=LINE('',#14218,#2976);
#2253=LINE('',#14224,#2977);
#2254=LINE('',#14230,#2978);
#2255=LINE('',#14235,#2979);
#2256=LINE('',#14239,#2980);
#2257=LINE('',#14240,#2981);
#2258=LINE('',#14244,#2982);
#2259=LINE('',#14248,#2983);
#2260=LINE('',#14249,#2984);
#2261=LINE('',#14252,#2985);
#2262=LINE('',#14253,#2986);
#2263=LINE('',#14255,#2987);
#2264=LINE('',#14256,#2988);
#2265=LINE('',#14260,#2989);
#2266=LINE('',#14262,#2990);
#2267=LINE('',#14264,#2991);
#2268=LINE('',#14265,#2992);
#2269=LINE('',#14269,#2993);
#2270=LINE('',#14272,#2994);
#2271=LINE('',#14273,#2995);
#2272=LINE('',#14276,#2996);
#2273=LINE('',#14280,#2997);
#2274=LINE('',#14281,#2998);
#2275=LINE('',#14285,#2999);
#2276=LINE('',#14289,#3000);
#2277=LINE('',#14293,#3001);
#2278=LINE('',#14295,#3002);
#2279=LINE('',#14296,#3003);
#2280=LINE('',#14300,#3004);
#2281=LINE('',#14304,#3005);
#2282=LINE('',#14308,#3006);
#2283=LINE('',#14310,#3007);
#2284=LINE('',#14311,#3008);
#2285=LINE('',#14318,#3009);
#2286=LINE('',#14322,#3010);
#2287=LINE('',#14323,#3011);
#2288=LINE('',#14327,#3012);
#2289=LINE('',#14332,#3013);
#2290=LINE('',#14334,#3014);
#2291=LINE('',#14335,#3015);
#2292=LINE('',#14340,#3016);
#2293=LINE('',#14345,#3017);
#2294=LINE('',#14350,#3018);
#2295=LINE('',#14352,#3019);
#2296=LINE('',#14353,#3020);
#2297=LINE('',#14357,#3021);
#2298=LINE('',#14361,#3022);
#2299=LINE('',#14364,#3023);
#2300=LINE('',#14365,#3024);
#2301=LINE('',#14369,#3025);
#2302=LINE('',#14374,#3026);
#2303=LINE('',#14376,#3027);
#2304=LINE('',#14377,#3028);
#2305=LINE('',#14381,#3029);
#2306=LINE('',#14385,#3030);
#2307=LINE('',#14388,#3031);
#2308=LINE('',#14389,#3032);
#2309=LINE('',#14392,#3033);
#2310=LINE('',#14393,#3034);
#2311=LINE('',#14394,#3035);
#2312=LINE('',#14397,#3036);
#2313=LINE('',#14398,#3037);
#2314=LINE('',#14400,#3038);
#2315=LINE('',#14401,#3039);
#2316=LINE('',#14403,#3040);
#2317=LINE('',#14405,#3041);
#2318=LINE('',#14407,#3042);
#2319=LINE('',#14409,#3043);
#2320=LINE('',#14412,#3044);
#2321=LINE('',#14414,#3045);
#2322=LINE('',#14416,#3046);
#2323=LINE('',#14419,#3047);
#2324=LINE('',#14420,#3048);
#2325=LINE('',#14423,#3049);
#2326=LINE('',#14424,#3050);
#2327=LINE('',#14426,#3051);
#2328=LINE('',#14427,#3052);
#2329=LINE('',#14429,#3053);
#2330=LINE('',#14431,#3054);
#2331=LINE('',#14433,#3055);
#2332=LINE('',#14434,#3056);
#2333=LINE('',#14436,#3057);
#2334=LINE('',#14437,#3058);
#2335=LINE('',#14438,#3059);
#2336=LINE('',#14440,#3060);
#2337=LINE('',#14442,#3061);
#2338=LINE('',#14444,#3062);
#2339=LINE('',#14452,#3063);
#2340=LINE('',#14459,#3064);
#2341=LINE('',#14461,#3065);
#2342=LINE('',#14463,#3066);
#2343=LINE('',#14466,#3067);
#2344=LINE('',#14468,#3068);
#2345=LINE('',#14469,#3069);
#2346=LINE('',#14472,#3070);
#2347=LINE('',#14474,#3071);
#2348=LINE('',#14475,#3072);
#2349=LINE('',#14478,#3073);
#2350=LINE('',#14480,#3074);
#2351=LINE('',#14481,#3075);
#2352=LINE('',#14484,#3076);
#2353=LINE('',#14486,#3077);
#2354=LINE('',#14487,#3078);
#2355=LINE('',#14489,#3079);
#2356=LINE('',#14491,#3080);
#2357=LINE('',#14498,#3081);
#2358=LINE('',#14504,#3082);
#2359=LINE('',#14506,#3083);
#2360=LINE('',#14508,#3084);
#2361=LINE('',#14511,#3085);
#2362=LINE('',#14513,#3086);
#2363=LINE('',#14514,#3087);
#2364=LINE('',#14517,#3088);
#2365=LINE('',#14519,#3089);
#2366=LINE('',#14520,#3090);
#2367=LINE('',#14523,#3091);
#2368=LINE('',#14525,#3092);
#2369=LINE('',#14526,#3093);
#2370=LINE('',#14529,#3094);
#2371=LINE('',#14531,#3095);
#2372=LINE('',#14532,#3096);
#2373=LINE('',#14534,#3097);
#2374=LINE('',#14536,#3098);
#2375=LINE('',#14543,#3099);
#2376=LINE('',#14549,#3100);
#2377=LINE('',#14555,#3101);
#2378=LINE('',#14561,#3102);
#2379=LINE('',#14567,#3103);
#2380=LINE('',#14573,#3104);
#2381=LINE('',#14579,#3105);
#2382=LINE('',#14585,#3106);
#2383=LINE('',#14590,#3107);
#2384=LINE('',#14592,#3108);
#2385=LINE('',#14594,#3109);
#2386=LINE('',#14595,#3110);
#2387=LINE('',#14599,#3111);
#2388=LINE('',#14603,#3112);
#2389=LINE('',#14607,#3113);
#2390=LINE('',#14609,#3114);
#2391=LINE('',#14610,#3115);
#2392=LINE('',#14614,#3116);
#2393=LINE('',#14618,#3117);
#2394=LINE('',#14622,#3118);
#2395=LINE('',#14624,#3119);
#2396=LINE('',#14625,#3120);
#2397=LINE('',#14629,#3121);
#2398=LINE('',#14633,#3122);
#2399=LINE('',#14636,#3123);
#2400=LINE('',#14637,#3124);
#2401=LINE('',#14644,#3125);
#2402=LINE('',#14645,#3126);
#2403=LINE('',#14646,#3127);
#2404=LINE('',#14650,#3128);
#2405=LINE('',#14652,#3129);
#2406=LINE('',#14654,#3130);
#2407=LINE('',#14655,#3131);
#2408=LINE('',#14658,#3132);
#2409=LINE('',#14660,#3133);
#2410=LINE('',#14661,#3134);
#2411=LINE('',#14664,#3135);
#2412=LINE('',#14666,#3136);
#2413=LINE('',#14667,#3137);
#2414=LINE('',#14672,#3138);
#2415=LINE('',#14676,#3139);
#2416=LINE('',#14677,#3140);
#2417=LINE('',#14678,#3141);
#2418=LINE('',#14680,#3142);
#2419=LINE('',#14681,#3143);
#2420=LINE('',#14683,#3144);
#2421=LINE('',#14685,#3145);
#2422=LINE('',#14687,#3146);
#2423=LINE('',#14690,#3147);
#2424=LINE('',#14691,#3148);
#2425=LINE('',#14694,#3149);
#2426=LINE('',#14695,#3150);
#2427=LINE('',#14697,#3151);
#2428=LINE('',#14698,#3152);
#2429=LINE('',#14700,#3153);
#2430=LINE('',#14702,#3154);
#2431=LINE('',#14704,#3155);
#2432=LINE('',#14707,#3156);
#2433=LINE('',#14709,#3157);
#2434=LINE('',#14711,#3158);
#2435=LINE('',#14713,#3159);
#2436=LINE('',#14714,#3160);
#2437=LINE('',#14720,#3161);
#2438=LINE('',#14723,#3162);
#2439=LINE('',#14730,#3163);
#2440=LINE('',#14736,#3164);
#2441=LINE('',#14742,#3165);
#2442=LINE('',#14748,#3166);
#2443=LINE('',#14754,#3167);
#2444=LINE('',#14760,#3168);
#2445=LINE('',#14766,#3169);
#2446=LINE('',#14772,#3170);
#2447=LINE('',#14777,#3171);
#2448=LINE('',#14779,#3172);
#2449=LINE('',#14781,#3173);
#2450=LINE('',#14782,#3174);
#2451=LINE('',#14786,#3175);
#2452=LINE('',#14790,#3176);
#2453=LINE('',#14794,#3177);
#2454=LINE('',#14796,#3178);
#2455=LINE('',#14797,#3179);
#2456=LINE('',#14801,#3180);
#2457=LINE('',#14805,#3181);
#2458=LINE('',#14809,#3182);
#2459=LINE('',#14811,#3183);
#2460=LINE('',#14812,#3184);
#2461=LINE('',#14816,#3185);
#2462=LINE('',#14820,#3186);
#2463=LINE('',#14823,#3187);
#2464=LINE('',#14824,#3188);
#2465=LINE('',#14831,#3189);
#2466=LINE('',#14832,#3190);
#2467=LINE('',#14833,#3191);
#2468=LINE('',#14837,#3192);
#2469=LINE('',#14839,#3193);
#2470=LINE('',#14841,#3194);
#2471=LINE('',#14842,#3195);
#2472=LINE('',#14845,#3196);
#2473=LINE('',#14847,#3197);
#2474=LINE('',#14848,#3198);
#2475=LINE('',#14851,#3199);
#2476=LINE('',#14853,#3200);
#2477=LINE('',#14854,#3201);
#2478=LINE('',#14860,#3202);
#2479=LINE('',#14863,#3203);
#2480=LINE('',#14865,#3204);
#2481=LINE('',#14866,#3205);
#2482=LINE('',#14867,#3206);
#2483=LINE('',#14868,#3207);
#2484=LINE('',#14870,#3208);
#2485=LINE('',#14872,#3209);
#2486=LINE('',#14874,#3210);
#2487=LINE('',#14877,#3211);
#2488=LINE('',#14878,#3212);
#2489=LINE('',#14881,#3213);
#2490=LINE('',#14882,#3214);
#2491=LINE('',#14884,#3215);
#2492=LINE('',#14885,#3216);
#2493=LINE('',#14887,#3217);
#2494=LINE('',#14889,#3218);
#2495=LINE('',#14891,#3219);
#2496=LINE('',#14894,#3220);
#2497=LINE('',#14896,#3221);
#2498=LINE('',#14898,#3222);
#2499=LINE('',#14900,#3223);
#2500=LINE('',#14901,#3224);
#2501=LINE('',#14907,#3225);
#2502=LINE('',#14910,#3226);
#2503=LINE('',#14917,#3227);
#2504=LINE('',#14923,#3228);
#2505=LINE('',#14929,#3229);
#2506=LINE('',#14934,#3230);
#2507=LINE('',#14938,#3231);
#2508=LINE('',#14942,#3232);
#2509=LINE('',#14944,#3233);
#2510=LINE('',#14945,#3234);
#2511=LINE('',#14949,#3235);
#2512=LINE('',#14953,#3236);
#2513=LINE('',#14957,#3237);
#2514=LINE('',#14959,#3238);
#2515=LINE('',#14960,#3239);
#2516=LINE('',#14964,#3240);
#2517=LINE('',#14969,#3241);
#2518=LINE('',#14971,#3242);
#2519=LINE('',#14972,#3243);
#2520=LINE('',#14976,#3244);
#2521=LINE('',#14980,#3245);
#2522=LINE('',#14983,#3246);
#2523=LINE('',#14984,#3247);
#2524=LINE('',#14988,#3248);
#2525=LINE('',#14994,#3249);
#2526=LINE('',#14995,#3250);
#2527=LINE('',#14996,#3251);
#2528=LINE('',#15000,#3252);
#2529=LINE('',#15004,#3253);
#2530=LINE('',#15007,#3254);
#2531=LINE('',#15008,#3255);
#2532=LINE('',#15012,#3256);
#2533=LINE('',#15013,#3257);
#2534=LINE('',#15014,#3258);
#2535=LINE('',#15018,#3259);
#2536=LINE('',#15020,#3260);
#2537=LINE('',#15022,#3261);
#2538=LINE('',#15023,#3262);
#2539=LINE('',#15026,#3263);
#2540=LINE('',#15028,#3264);
#2541=LINE('',#15029,#3265);
#2542=LINE('',#15032,#3266);
#2543=LINE('',#15034,#3267);
#2544=LINE('',#15035,#3268);
#2545=LINE('',#15041,#3269);
#2546=LINE('',#15044,#3270);
#2547=LINE('',#15046,#3271);
#2548=LINE('',#15047,#3272);
#2549=LINE('',#15048,#3273);
#2550=LINE('',#15049,#3274);
#2551=LINE('',#15051,#3275);
#2552=LINE('',#15053,#3276);
#2553=LINE('',#15055,#3277);
#2554=LINE('',#15057,#3278);
#2555=LINE('',#15059,#3279);
#2556=LINE('',#15062,#3280);
#2557=LINE('',#15063,#3281);
#2558=LINE('',#15066,#3282);
#2559=LINE('',#15067,#3283);
#2560=LINE('',#15069,#3284);
#2561=LINE('',#15070,#3285);
#2562=LINE('',#15072,#3286);
#2563=LINE('',#15074,#3287);
#2564=LINE('',#15076,#3288);
#2565=LINE('',#15078,#3289);
#2566=LINE('',#15080,#3290);
#2567=LINE('',#15084,#3291);
#2568=LINE('',#15086,#3292);
#2569=LINE('',#15087,#3293);
#2570=LINE('',#15089,#3294);
#2571=LINE('',#15090,#3295);
#2572=LINE('',#15096,#3296);
#2573=LINE('',#15099,#3297);
#2574=LINE('',#15105,#3298);
#2575=LINE('',#15109,#3299);
#2576=LINE('',#15113,#3300);
#2577=LINE('',#15115,#3301);
#2578=LINE('',#15116,#3302);
#2579=LINE('',#15120,#3303);
#2580=LINE('',#15124,#3304);
#2581=LINE('',#15128,#3305);
#2582=LINE('',#15130,#3306);
#2583=LINE('',#15131,#3307);
#2584=LINE('',#15135,#3308);
#2585=LINE('',#15140,#3309);
#2586=LINE('',#15142,#3310);
#2587=LINE('',#15143,#3311);
#2588=LINE('',#15147,#3312);
#2589=LINE('',#15151,#3313);
#2590=LINE('',#15154,#3314);
#2591=LINE('',#15155,#3315);
#2592=LINE('',#15158,#3316);
#2593=LINE('',#15159,#3317);
#2594=LINE('',#15160,#3318);
#2595=LINE('',#15163,#3319);
#2596=LINE('',#15164,#3320);
#2597=LINE('',#15166,#3321);
#2598=LINE('',#15167,#3322);
#2599=LINE('',#15169,#3323);
#2600=LINE('',#15171,#3324);
#2601=LINE('',#15173,#3325);
#2602=LINE('',#15176,#3326);
#2603=LINE('',#15177,#3327);
#2604=LINE('',#15180,#3328);
#2605=LINE('',#15181,#3329);
#2606=LINE('',#15183,#3330);
#2607=LINE('',#15184,#3331);
#2608=LINE('',#15186,#3332);
#2609=LINE('',#15188,#3333);
#2610=LINE('',#15234,#3334);
#2611=LINE('',#15235,#3335);
#2612=LINE('',#15847,#3336);
#2613=LINE('',#15861,#3337);
#2614=LINE('',#15878,#3338);
#2615=LINE('',#15892,#3339);
#2616=LINE('',#15895,#3340);
#2617=LINE('',#15909,#3341);
#2618=LINE('',#15912,#3342);
#2619=LINE('',#15926,#3343);
#2620=LINE('',#15943,#3344);
#2621=LINE('',#15957,#3345);
#2622=LINE('',#15960,#3346);
#2623=LINE('',#15974,#3347);
#2624=LINE('',#15977,#3348);
#2625=LINE('',#15991,#3349);
#2626=LINE('',#15994,#3350);
#2627=LINE('',#16008,#3351);
#2628=LINE('',#16011,#3352);
#2629=LINE('',#16025,#3353);
#2630=LINE('',#16028,#3354);
#2631=LINE('',#16042,#3355);
#2632=LINE('',#16047,#3356);
#2633=LINE('',#16086,#3357);
#2634=LINE('',#16089,#3358);
#2635=LINE('',#16094,#3359);
#2636=LINE('',#16100,#3360);
#2637=LINE('',#16104,#3361);
#2638=LINE('',#16106,#3362);
#2639=LINE('',#16107,#3363);
#2640=LINE('',#16109,#3364);
#2641=LINE('',#16111,#3365);
#2642=LINE('',#16112,#3366);
#2643=LINE('',#16116,#3367);
#2644=LINE('',#16118,#3368);
#2645=LINE('',#16122,#3369);
#2646=LINE('',#16126,#3370);
#2647=LINE('',#16128,#3371);
#2648=LINE('',#16130,#3372);
#2649=LINE('',#16134,#3373);
#2650=LINE('',#16137,#3374);
#2651=LINE('',#16145,#3375);
#2652=LINE('',#16146,#3376);
#2653=LINE('',#16148,#3377);
#2654=LINE('',#16150,#3378);
#2655=LINE('',#16152,#3379);
#2656=LINE('',#16153,#3380);
#2657=LINE('',#16155,#3381);
#2658=LINE('',#16156,#3382);
#2659=LINE('',#16162,#3383);
#2660=LINE('',#16195,#3384);
#2661=LINE('',#16200,#3385);
#2662=LINE('',#16248,#3386);
#2663=LINE('',#16253,#3387);
#2664=LINE('',#16255,#3388);
#2665=LINE('',#16268,#3389);
#2666=LINE('',#16270,#3390);
#2667=LINE('',#16286,#3391);
#2668=LINE('',#16337,#3392);
#2669=LINE('',#16340,#3393);
#2670=LINE('',#16344,#3394);
#2671=LINE('',#16350,#3395);
#2672=LINE('',#16383,#3396);
#2673=LINE('',#16390,#3397);
#2674=LINE('',#16392,#3398);
#2675=LINE('',#16408,#3399);
#2676=LINE('',#16410,#3400);
#2677=LINE('',#16423,#3401);
#2678=LINE('',#16427,#3402);
#2679=LINE('',#16446,#3403);
#2680=LINE('',#16448,#3404);
#2681=LINE('',#16461,#3405);
#2682=LINE('',#16463,#3406);
#2683=LINE('',#16479,#3407);
#2684=LINE('',#16481,#3408);
#2685=LINE('',#16624,#3409);
#2686=LINE('',#16629,#3410);
#2687=LINE('',#16663,#3411);
#2688=LINE('',#16667,#3412);
#2689=LINE('',#16719,#3413);
#2690=LINE('',#16723,#3414);
#2691=LINE('',#16762,#3415);
#2692=LINE('',#16764,#3416);
#2693=LINE('',#16777,#3417);
#2694=LINE('',#16779,#3418);
#2695=LINE('',#16795,#3419);
#2696=LINE('',#16810,#3420);
#2697=LINE('',#16813,#3421);
#2698=LINE('',#16817,#3422);
#2699=LINE('',#16823,#3423);
#2700=LINE('',#16835,#3424);
#2701=LINE('',#16842,#3425);
#2702=LINE('',#16854,#3426);
#2703=LINE('',#16859,#3427);
#2704=LINE('',#16861,#3428);
#2705=LINE('',#16878,#3429);
#2706=LINE('',#16882,#3430);
#2707=LINE('',#16891,#3431);
#2708=LINE('',#16893,#3432);
#2709=LINE('',#16906,#3433);
#2710=LINE('',#16908,#3434);
#2711=LINE('',#16924,#3435);
#2712=LINE('',#16939,#3436);
#2713=LINE('',#16942,#3437);
#2714=LINE('',#16946,#3438);
#2715=LINE('',#16952,#3439);
#2716=LINE('',#16964,#3440);
#2717=LINE('',#16969,#3441);
#2718=LINE('',#16971,#3442);
#2719=LINE('',#16975,#3443);
#2720=LINE('',#16981,#3444);
#2721=LINE('',#16990,#3445);
#2722=LINE('',#16992,#3446);
#2723=LINE('',#16996,#3447);
#2724=LINE('',#17000,#3448);
#2725=LINE('',#17010,#3449);
#2726=LINE('',#17079,#3450);
#2727=LINE('',#17085,#3451);
#2728=LINE('',#17115,#3452);
#2729=LINE('',#17121,#3453);
#2730=LINE('',#17190,#3454);
#2731=LINE('',#17240,#3455);
#2732=LINE('',#17242,#3456);
#2733=LINE('',#17243,#3457);
#2734=LINE('',#17245,#3458);
#2735=LINE('',#17246,#3459);
#2736=LINE('',#17248,#3460);
#2737=LINE('',#17264,#3461);
#2738=LINE('',#17275,#3462);
#2739=LINE('',#17279,#3463);
#2740=LINE('',#17344,#3464);
#2741=LINE('',#17346,#3465);
#2742=LINE('',#17347,#3466);
#2743=LINE('',#17350,#3467);
#2744=LINE('',#17351,#3468);
#2745=LINE('',#17354,#3469);
#2746=LINE('',#17355,#3470);
#2747=LINE('',#17358,#3471);
#2748=LINE('',#17359,#3472);
#2749=LINE('',#17362,#3473);
#2750=LINE('',#17363,#3474);
#2751=LINE('',#17365,#3475);
#2752=LINE('',#17374,#3476);
#2753=LINE('',#17389,#3477);
#2754=LINE('',#17394,#3478);
#2755=LINE('',#17404,#3479);
#2756=LINE('',#17428,#3480);
#2757=LINE('',#17446,#3481);
#2758=LINE('',#17463,#3482);
#2759=LINE('',#17468,#3483);
#2760=LINE('',#17472,#3484);
#2761=LINE('',#17537,#3485);
#2762=LINE('',#17538,#3486);
#2763=LINE('',#17540,#3487);
#2764=LINE('',#17541,#3488);
#2765=LINE('',#17544,#3489);
#2766=LINE('',#17545,#3490);
#2767=LINE('',#17546,#3491);
#2768=LINE('',#17549,#3492);
#2769=LINE('',#17550,#3493);
#2770=LINE('',#17551,#3494);
#2771=LINE('',#17554,#3495);
#2772=LINE('',#17555,#3496);
#2773=LINE('',#17556,#3497);
#2774=LINE('',#17559,#3498);
#2775=LINE('',#17560,#3499);
#2776=LINE('',#17561,#3500);
#2777=LINE('',#17563,#3501);
#2778=LINE('',#17564,#3502);
#2779=LINE('',#17587,#3503);
#2780=LINE('',#17589,#3504);
#2781=LINE('',#17592,#3505);
#2782=LINE('',#17597,#3506);
#2783=LINE('',#17602,#3507);
#2784=LINE('',#17612,#3508);
#2785=LINE('',#17616,#3509);
#2786=LINE('',#17627,#3510);
#2787=LINE('',#17631,#3511);
#2788=LINE('',#17642,#3512);
#2789=LINE('',#17646,#3513);
#2790=LINE('',#17648,#3514);
#2791=LINE('',#17650,#3515);
#2792=LINE('',#17674,#3516);
#2793=LINE('',#17685,#3517);
#2794=LINE('',#17710,#3518);
#2795=LINE('',#17719,#3519);
#2796=LINE('',#17721,#3520);
#2797=LINE('',#17723,#3521);
#2798=LINE('',#17724,#3522);
#2799=LINE('',#17727,#3523);
#2800=LINE('',#17729,#3524);
#2801=LINE('',#17730,#3525);
#2802=LINE('',#17733,#3526);
#2803=LINE('',#17735,#3527);
#2804=LINE('',#17736,#3528);
#2805=LINE('',#17739,#3529);
#2806=LINE('',#17741,#3530);
#2807=LINE('',#17742,#3531);
#2808=LINE('',#17745,#3532);
#2809=LINE('',#17747,#3533);
#2810=LINE('',#17748,#3534);
#2811=LINE('',#17751,#3535);
#2812=LINE('',#17753,#3536);
#2813=LINE('',#17754,#3537);
#2814=LINE('',#17757,#3538);
#2815=LINE('',#17759,#3539);
#2816=LINE('',#17760,#3540);
#2817=LINE('',#17762,#3541);
#2818=LINE('',#17763,#3542);
#2819=LINE('',#17773,#3543);
#2820=LINE('',#17779,#3544);
#2821=LINE('',#17785,#3545);
#2822=LINE('',#17796,#3546);
#2823=LINE('',#17805,#3547);
#2824=LINE('',#17811,#3548);
#2825=LINE('',#17817,#3549);
#2826=LINE('',#17823,#3550);
#2827=LINE('',#17838,#3551);
#2828=LINE('',#17848,#3552);
#2829=LINE('',#17858,#3553);
#2830=LINE('',#17872,#3554);
#2831=LINE('',#17884,#3555);
#2832=LINE('',#17888,#3556);
#2833=LINE('',#17896,#3557);
#2834=LINE('',#17911,#3558);
#2835=LINE('',#17917,#3559);
#2836=LINE('',#17927,#3560);
#2837=LINE('',#17932,#3561);
#2838=LINE('',#17936,#3562);
#2839=LINE('',#17942,#3563);
#2840=VECTOR('',#10869,6.00000000000002);
#2841=VECTOR('',#10876,6.00000000000001);
#2842=VECTOR('',#10883,6.00000000000002);
#2843=VECTOR('',#10890,6.00000000000001);
#2844=VECTOR('',#10897,6.34999999999999);
#2845=VECTOR('',#10904,6.35000000000122);
#2846=VECTOR('',#10911,6.35000000000122);
#2847=VECTOR('',#10918,6.46290152238551);
#2848=VECTOR('',#10925,6.4629015223855);
#2849=VECTOR('',#10932,6.34999999999994);
#2850=VECTOR('',#10939,6.34999999999994);
#2851=VECTOR('',#10944,1000.);
#2852=VECTOR('',#10947,1000.);
#2853=VECTOR('',#10948,1000.);
#2854=VECTOR('',#10951,1000.);
#2855=VECTOR('',#10954,1000.);
#2856=VECTOR('',#10955,1000.);
#2857=VECTOR('',#10958,1000.);
#2858=VECTOR('',#10959,1000.);
#2859=VECTOR('',#10960,1000.);
#2860=VECTOR('',#10961,1000.);
#2861=VECTOR('',#10964,1000.);
#2862=VECTOR('',#10965,1000.);
#2863=VECTOR('',#10966,1000.);
#2864=VECTOR('',#10967,1000.);
#2865=VECTOR('',#10970,1000.);
#2866=VECTOR('',#10973,1000.);
#2867=VECTOR('',#10974,1000.);
#2868=VECTOR('',#10977,1000.);
#2869=VECTOR('',#10980,1000.);
#2870=VECTOR('',#10981,1000.);
#2871=VECTOR('',#10984,1000.);
#2872=VECTOR('',#10987,1000.);
#2873=VECTOR('',#10992,1000.);
#2874=VECTOR('',#10993,1000.);
#2875=VECTOR('',#10994,1000.);
#2876=VECTOR('',#10997,1000.);
#2877=VECTOR('',#11000,1000.);
#2878=VECTOR('',#11005,1000.);
#2879=VECTOR('',#11006,1000.);
#2880=VECTOR('',#11007,1000.);
#2881=VECTOR('',#11010,1000.);
#2882=VECTOR('',#11017,1000.);
#2883=VECTOR('',#11018,1000.);
#2884=VECTOR('',#11019,1000.);
#2885=VECTOR('',#11022,1000.);
#2886=VECTOR('',#11025,1000.);
#2887=VECTOR('',#11030,1000.);
#2888=VECTOR('',#11031,1000.);
#2889=VECTOR('',#11040,1000.);
#2890=VECTOR('',#11047,1000.);
#2891=VECTOR('',#11048,1000.);
#2892=VECTOR('',#11051,1000.);
#2893=VECTOR('',#11058,1000.);
#2894=VECTOR('',#11059,1000.);
#2895=VECTOR('',#11060,1000.);
#2896=VECTOR('',#11065,1000.);
#2897=VECTOR('',#11070,1000.);
#2898=VECTOR('',#11077,1000.);
#2899=VECTOR('',#11078,1000.);
#2900=VECTOR('',#11079,1000.);
#2901=VECTOR('',#11082,1000.);
#2902=VECTOR('',#11085,1000.);
#2903=VECTOR('',#11090,1000.);
#2904=VECTOR('',#11091,1000.);
#2905=VECTOR('',#11094,1000.);
#2906=VECTOR('',#11095,1000.);
#2907=VECTOR('',#11096,1000.);
#2908=VECTOR('',#11099,1000.);
#2909=VECTOR('',#11100,1000.);
#2910=VECTOR('',#11103,1000.);
#2911=VECTOR('',#11104,1000.);
#2912=VECTOR('',#11107,1000.);
#2913=VECTOR('',#11110,1000.);
#2914=VECTOR('',#11115,1000.);
#2915=VECTOR('',#11118,1000.);
#2916=VECTOR('',#11121,1000.);
#2917=VECTOR('',#11124,1000.);
#2918=VECTOR('',#11127,1000.);
#2919=VECTOR('',#11130,1000.);
#2920=VECTOR('',#11131,1000.);
#2921=VECTOR('',#11134,1000.);
#2922=VECTOR('',#11135,1000.);
#2923=VECTOR('',#11138,1000.);
#2924=VECTOR('',#11139,1000.);
#2925=VECTOR('',#11142,1000.);
#2926=VECTOR('',#11145,1000.);
#2927=VECTOR('',#11148,1000.);
#2928=VECTOR('',#11151,1000.);
#2929=VECTOR('',#11154,1000.);
#2930=VECTOR('',#11155,1000.);
#2931=VECTOR('',#11158,1000.);
#2932=VECTOR('',#11159,1000.);
#2933=VECTOR('',#11160,1000.);
#2934=VECTOR('',#11163,1000.);
#2935=VECTOR('',#11174,1000.);
#2936=VECTOR('',#11183,1000.);
#2937=VECTOR('',#11186,1000.);
#2938=VECTOR('',#11189,1000.);
#2939=VECTOR('',#11192,1000.);
#2940=VECTOR('',#11193,1000.);
#2941=VECTOR('',#11194,1000.);
#2942=VECTOR('',#11197,1000.);
#2943=VECTOR('',#11198,1000.);
#2944=VECTOR('',#11199,1000.);
#2945=VECTOR('',#11202,1000.);
#2946=VECTOR('',#11203,1000.);
#2947=VECTOR('',#11204,1000.);
#2948=VECTOR('',#11207,1000.);
#2949=VECTOR('',#11208,1000.);
#2950=VECTOR('',#11209,1000.);
#2951=VECTOR('',#11212,1000.);
#2952=VECTOR('',#11215,1000.);
#2953=VECTOR('',#11224,1000.);
#2954=VECTOR('',#11231,1000.);
#2955=VECTOR('',#11234,1000.);
#2956=VECTOR('',#11237,1000.);
#2957=VECTOR('',#11240,1000.);
#2958=VECTOR('',#11241,1000.);
#2959=VECTOR('',#11242,1000.);
#2960=VECTOR('',#11245,1000.);
#2961=VECTOR('',#11246,1000.);
#2962=VECTOR('',#11247,1000.);
#2963=VECTOR('',#11250,1000.);
#2964=VECTOR('',#11251,1000.);
#2965=VECTOR('',#11252,1000.);
#2966=VECTOR('',#11255,1000.);
#2967=VECTOR('',#11256,1000.);
#2968=VECTOR('',#11257,1000.);
#2969=VECTOR('',#11260,1000.);
#2970=VECTOR('',#11263,1000.);
#2971=VECTOR('',#11272,6.00000000000001);
#2972=VECTOR('',#11279,6.00000000000001);
#2973=VECTOR('',#11286,6.00000000000001);
#2974=VECTOR('',#11293,6.00000000000001);
#2975=VECTOR('',#11300,6.34999999999994);
#2976=VECTOR('',#11307,6.34999999999997);
#2977=VECTOR('',#11314,6.34999999999995);
#2978=VECTOR('',#11321,6.34999999999997);
#2979=VECTOR('',#11326,1000.);
#2980=VECTOR('',#11329,1000.);
#2981=VECTOR('',#11330,1000.);
#2982=VECTOR('',#11333,1000.);
#2983=VECTOR('',#11336,1000.);
#2984=VECTOR('',#11337,1000.);
#2985=VECTOR('',#11340,1000.);
#2986=VECTOR('',#11341,1000.);
#2987=VECTOR('',#11342,1000.);
#2988=VECTOR('',#11343,1000.);
#2989=VECTOR('',#11346,1000.);
#2990=VECTOR('',#11347,1000.);
#2991=VECTOR('',#11348,1000.);
#2992=VECTOR('',#11349,1000.);
#2993=VECTOR('',#11352,1000.);
#2994=VECTOR('',#11355,1000.);
#2995=VECTOR('',#11356,1000.);
#2996=VECTOR('',#11359,1000.);
#2997=VECTOR('',#11362,1000.);
#2998=VECTOR('',#11363,1000.);
#2999=VECTOR('',#11366,1000.);
#3000=VECTOR('',#11369,1000.);
#3001=VECTOR('',#11374,1000.);
#3002=VECTOR('',#11375,1000.);
#3003=VECTOR('',#11376,1000.);
#3004=VECTOR('',#11379,1000.);
#3005=VECTOR('',#11382,1000.);
#3006=VECTOR('',#11387,1000.);
#3007=VECTOR('',#11388,1000.);
#3008=VECTOR('',#11389,1000.);
#3009=VECTOR('',#11398,1000.);
#3010=VECTOR('',#11405,1000.);
#3011=VECTOR('',#11406,1000.);
#3012=VECTOR('',#11409,1000.);
#3013=VECTOR('',#11416,1000.);
#3014=VECTOR('',#11417,1000.);
#3015=VECTOR('',#11418,1000.);
#3016=VECTOR('',#11423,1000.);
#3017=VECTOR('',#11428,1000.);
#3018=VECTOR('',#11435,1000.);
#3019=VECTOR('',#11436,1000.);
#3020=VECTOR('',#11437,1000.);
#3021=VECTOR('',#11440,1000.);
#3022=VECTOR('',#11443,1000.);
#3023=VECTOR('',#11448,1000.);
#3024=VECTOR('',#11449,1000.);
#3025=VECTOR('',#11452,1000.);
#3026=VECTOR('',#11459,1000.);
#3027=VECTOR('',#11460,1000.);
#3028=VECTOR('',#11461,1000.);
#3029=VECTOR('',#11464,1000.);
#3030=VECTOR('',#11467,1000.);
#3031=VECTOR('',#11472,1000.);
#3032=VECTOR('',#11473,1000.);
#3033=VECTOR('',#11476,1000.);
#3034=VECTOR('',#11477,1000.);
#3035=VECTOR('',#11478,1000.);
#3036=VECTOR('',#11481,1000.);
#3037=VECTOR('',#11482,1000.);
#3038=VECTOR('',#11485,1000.);
#3039=VECTOR('',#11486,1000.);
#3040=VECTOR('',#11489,1000.);
#3041=VECTOR('',#11492,1000.);
#3042=VECTOR('',#11495,1000.);
#3043=VECTOR('',#11498,1000.);
#3044=VECTOR('',#11503,1000.);
#3045=VECTOR('',#11506,1000.);
#3046=VECTOR('',#11509,1000.);
#3047=VECTOR('',#11512,1000.);
#3048=VECTOR('',#11513,1000.);
#3049=VECTOR('',#11516,1000.);
#3050=VECTOR('',#11517,1000.);
#3051=VECTOR('',#11520,1000.);
#3052=VECTOR('',#11521,1000.);
#3053=VECTOR('',#11524,1000.);
#3054=VECTOR('',#11527,1000.);
#3055=VECTOR('',#11530,1000.);
#3056=VECTOR('',#11531,1000.);
#3057=VECTOR('',#11534,1000.);
#3058=VECTOR('',#11535,1000.);
#3059=VECTOR('',#11536,1000.);
#3060=VECTOR('',#11539,1000.);
#3061=VECTOR('',#11542,1000.);
#3062=VECTOR('',#11545,1000.);
#3063=VECTOR('',#11556,1000.);
#3064=VECTOR('',#11565,1000.);
#3065=VECTOR('',#11568,1000.);
#3066=VECTOR('',#11571,1000.);
#3067=VECTOR('',#11574,1000.);
#3068=VECTOR('',#11575,1000.);
#3069=VECTOR('',#11576,1000.);
#3070=VECTOR('',#11579,1000.);
#3071=VECTOR('',#11580,1000.);
#3072=VECTOR('',#11581,1000.);
#3073=VECTOR('',#11584,1000.);
#3074=VECTOR('',#11585,1000.);
#3075=VECTOR('',#11586,1000.);
#3076=VECTOR('',#11589,1000.);
#3077=VECTOR('',#11590,1000.);
#3078=VECTOR('',#11591,1000.);
#3079=VECTOR('',#11594,1000.);
#3080=VECTOR('',#11597,1000.);
#3081=VECTOR('',#11606,1000.);
#3082=VECTOR('',#11613,1000.);
#3083=VECTOR('',#11616,1000.);
#3084=VECTOR('',#11619,1000.);
#3085=VECTOR('',#11622,1000.);
#3086=VECTOR('',#11623,1000.);
#3087=VECTOR('',#11624,1000.);
#3088=VECTOR('',#11627,1000.);
#3089=VECTOR('',#11628,1000.);
#3090=VECTOR('',#11629,1000.);
#3091=VECTOR('',#11632,1000.);
#3092=VECTOR('',#11633,1000.);
#3093=VECTOR('',#11634,1000.);
#3094=VECTOR('',#11637,1000.);
#3095=VECTOR('',#11638,1000.);
#3096=VECTOR('',#11639,1000.);
#3097=VECTOR('',#11642,1000.);
#3098=VECTOR('',#11645,1000.);
#3099=VECTOR('',#11654,6.34999999871023);
#3100=VECTOR('',#11661,6.34999999871025);
#3101=VECTOR('',#11668,6.34999999999997);
#3102=VECTOR('',#11675,6.98053323984749);
#3103=VECTOR('',#11682,6.35);
#3104=VECTOR('',#11689,6.34999999999999);
#3105=VECTOR('',#11696,6.35);
#3106=VECTOR('',#11703,6.35);
#3107=VECTOR('',#11708,1000.);
#3108=VECTOR('',#11709,1000.);
#3109=VECTOR('',#11710,1000.);
#3110=VECTOR('',#11711,1000.);
#3111=VECTOR('',#11714,1000.);
#3112=VECTOR('',#11717,1000.);
#3113=VECTOR('',#11722,1000.);
#3114=VECTOR('',#11723,1000.);
#3115=VECTOR('',#11724,1000.);
#3116=VECTOR('',#11727,1000.);
#3117=VECTOR('',#11730,1000.);
#3118=VECTOR('',#11735,1000.);
#3119=VECTOR('',#11736,1000.);
#3120=VECTOR('',#11737,1000.);
#3121=VECTOR('',#11740,1000.);
#3122=VECTOR('',#11743,1000.);
#3123=VECTOR('',#11748,1000.);
#3124=VECTOR('',#11749,1000.);
#3125=VECTOR('',#11758,1000.);
#3126=VECTOR('',#11759,1000.);
#3127=VECTOR('',#11760,1000.);
#3128=VECTOR('',#11763,1000.);
#3129=VECTOR('',#11764,1000.);
#3130=VECTOR('',#11765,1000.);
#3131=VECTOR('',#11766,1000.);
#3132=VECTOR('',#11769,1000.);
#3133=VECTOR('',#11770,1000.);
#3134=VECTOR('',#11771,1000.);
#3135=VECTOR('',#11774,1000.);
#3136=VECTOR('',#11775,1000.);
#3137=VECTOR('',#11776,1000.);
#3138=VECTOR('',#11781,1000.);
#3139=VECTOR('',#11786,1000.);
#3140=VECTOR('',#11787,1000.);
#3141=VECTOR('',#11788,1000.);
#3142=VECTOR('',#11789,1000.);
#3143=VECTOR('',#11790,1000.);
#3144=VECTOR('',#11793,1000.);
#3145=VECTOR('',#11796,1000.);
#3146=VECTOR('',#11799,1000.);
#3147=VECTOR('',#11802,1000.);
#3148=VECTOR('',#11803,1000.);
#3149=VECTOR('',#11806,1000.);
#3150=VECTOR('',#11807,1000.);
#3151=VECTOR('',#11810,1000.);
#3152=VECTOR('',#11811,1000.);
#3153=VECTOR('',#11814,1000.);
#3154=VECTOR('',#11817,1000.);
#3155=VECTOR('',#11820,1000.);
#3156=VECTOR('',#11823,1000.);
#3157=VECTOR('',#11824,1000.);
#3158=VECTOR('',#11825,1000.);
#3159=VECTOR('',#11826,1000.);
#3160=VECTOR('',#11827,1000.);
#3161=VECTOR('',#11838,1000.);
#3162=VECTOR('',#11843,1000.);
#3163=VECTOR('',#11852,7.11098481470124);
#3164=VECTOR('',#11859,6.34999999871023);
#3165=VECTOR('',#11866,6.34999999999997);
#3166=VECTOR('',#11873,6.98053323984749);
#3167=VECTOR('',#11880,6.35);
#3168=VECTOR('',#11887,6.34999999999999);
#3169=VECTOR('',#11894,6.35);
#3170=VECTOR('',#11901,6.35);
#3171=VECTOR('',#11906,1000.);
#3172=VECTOR('',#11907,1000.);
#3173=VECTOR('',#11908,1000.);
#3174=VECTOR('',#11909,1000.);
#3175=VECTOR('',#11912,1000.);
#3176=VECTOR('',#11915,1000.);
#3177=VECTOR('',#11920,1000.);
#3178=VECTOR('',#11921,1000.);
#3179=VECTOR('',#11922,1000.);
#3180=VECTOR('',#11925,1000.);
#3181=VECTOR('',#11928,1000.);
#3182=VECTOR('',#11933,1000.);
#3183=VECTOR('',#11934,1000.);
#3184=VECTOR('',#11935,1000.);
#3185=VECTOR('',#11938,1000.);
#3186=VECTOR('',#11941,1000.);
#3187=VECTOR('',#11946,1000.);
#3188=VECTOR('',#11947,1000.);
#3189=VECTOR('',#11956,1000.);
#3190=VECTOR('',#11957,1000.);
#3191=VECTOR('',#11958,1000.);
#3192=VECTOR('',#11961,1000.);
#3193=VECTOR('',#11962,1000.);
#3194=VECTOR('',#11963,1000.);
#3195=VECTOR('',#11964,1000.);
#3196=VECTOR('',#11967,1000.);
#3197=VECTOR('',#11968,1000.);
#3198=VECTOR('',#11969,1000.);
#3199=VECTOR('',#11972,1000.);
#3200=VECTOR('',#11973,1000.);
#3201=VECTOR('',#11974,1000.);
#3202=VECTOR('',#11981,1000.);
#3203=VECTOR('',#11984,1000.);
#3204=VECTOR('',#11985,1000.);
#3205=VECTOR('',#11986,1000.);
#3206=VECTOR('',#11987,1000.);
#3207=VECTOR('',#11988,1000.);
#3208=VECTOR('',#11991,1000.);
#3209=VECTOR('',#11994,1000.);
#3210=VECTOR('',#11997,1000.);
#3211=VECTOR('',#12000,1000.);
#3212=VECTOR('',#12001,1000.);
#3213=VECTOR('',#12004,1000.);
#3214=VECTOR('',#12005,1000.);
#3215=VECTOR('',#12008,1000.);
#3216=VECTOR('',#12009,1000.);
#3217=VECTOR('',#12012,1000.);
#3218=VECTOR('',#12015,1000.);
#3219=VECTOR('',#12018,1000.);
#3220=VECTOR('',#12021,1000.);
#3221=VECTOR('',#12022,1000.);
#3222=VECTOR('',#12023,1000.);
#3223=VECTOR('',#12024,1000.);
#3224=VECTOR('',#12025,1000.);
#3225=VECTOR('',#12036,1000.);
#3226=VECTOR('',#12041,1000.);
#3227=VECTOR('',#12050,6.34999999999999);
#3228=VECTOR('',#12057,6.34999999999999);
#3229=VECTOR('',#12064,6.35);
#3230=VECTOR('',#12069,1000.);
#3231=VECTOR('',#12072,1000.);
#3232=VECTOR('',#12077,1000.);
#3233=VECTOR('',#12078,1000.);
#3234=VECTOR('',#12079,1000.);
#3235=VECTOR('',#12082,1000.);
#3236=VECTOR('',#12085,1000.);
#3237=VECTOR('',#12090,1000.);
#3238=VECTOR('',#12091,1000.);
#3239=VECTOR('',#12092,1000.);
#3240=VECTOR('',#12095,1000.);
#3241=VECTOR('',#12102,1000.);
#3242=VECTOR('',#12103,1000.);
#3243=VECTOR('',#12104,1000.);
#3244=VECTOR('',#12107,1000.);
#3245=VECTOR('',#12110,1000.);
#3246=VECTOR('',#12115,1000.);
#3247=VECTOR('',#12116,1000.);
#3248=VECTOR('',#12119,1000.);
#3249=VECTOR('',#12126,1000.);
#3250=VECTOR('',#12127,1000.);
#3251=VECTOR('',#12128,1000.);
#3252=VECTOR('',#12131,1000.);
#3253=VECTOR('',#12134,1000.);
#3254=VECTOR('',#12139,1000.);
#3255=VECTOR('',#12140,1000.);
#3256=VECTOR('',#12143,1000.);
#3257=VECTOR('',#12144,1000.);
#3258=VECTOR('',#12145,1000.);
#3259=VECTOR('',#12148,1000.);
#3260=VECTOR('',#12149,1000.);
#3261=VECTOR('',#12150,1000.);
#3262=VECTOR('',#12151,1000.);
#3263=VECTOR('',#12154,1000.);
#3264=VECTOR('',#12155,1000.);
#3265=VECTOR('',#12156,1000.);
#3266=VECTOR('',#12159,1000.);
#3267=VECTOR('',#12160,1000.);
#3268=VECTOR('',#12161,1000.);
#3269=VECTOR('',#12168,1000.);
#3270=VECTOR('',#12171,1000.);
#3271=VECTOR('',#12172,1000.);
#3272=VECTOR('',#12173,1000.);
#3273=VECTOR('',#12174,1000.);
#3274=VECTOR('',#12175,1000.);
#3275=VECTOR('',#12178,1000.);
#3276=VECTOR('',#12181,1000.);
#3277=VECTOR('',#12184,1000.);
#3278=VECTOR('',#12187,1000.);
#3279=VECTOR('',#12190,1000.);
#3280=VECTOR('',#12193,1000.);
#3281=VECTOR('',#12194,1000.);
#3282=VECTOR('',#12197,1000.);
#3283=VECTOR('',#12198,1000.);
#3284=VECTOR('',#12201,1000.);
#3285=VECTOR('',#12202,1000.);
#3286=VECTOR('',#12205,1000.);
#3287=VECTOR('',#12208,1000.);
#3288=VECTOR('',#12211,1000.);
#3289=VECTOR('',#12214,1000.);
#3290=VECTOR('',#12217,1000.);
#3291=VECTOR('',#12220,1000.);
#3292=VECTOR('',#12221,1000.);
#3293=VECTOR('',#12222,1000.);
#3294=VECTOR('',#12223,1000.);
#3295=VECTOR('',#12224,1000.);
#3296=VECTOR('',#12235,1000.);
#3297=VECTOR('',#12240,1000.);
#3298=VECTOR('',#12247,1000.);
#3299=VECTOR('',#12250,1000.);
#3300=VECTOR('',#12255,1000.);
#3301=VECTOR('',#12256,1000.);
#3302=VECTOR('',#12257,1000.);
#3303=VECTOR('',#12260,1000.);
#3304=VECTOR('',#12263,1000.);
#3305=VECTOR('',#12268,1000.);
#3306=VECTOR('',#12269,1000.);
#3307=VECTOR('',#12270,1000.);
#3308=VECTOR('',#12273,1000.);
#3309=VECTOR('',#12280,1000.);
#3310=VECTOR('',#12281,1000.);
#3311=VECTOR('',#12282,1000.);
#3312=VECTOR('',#12285,1000.);
#3313=VECTOR('',#12288,1000.);
#3314=VECTOR('',#12293,1000.);
#3315=VECTOR('',#12294,1000.);
#3316=VECTOR('',#12297,1000.);
#3317=VECTOR('',#12298,1000.);
#3318=VECTOR('',#12299,1000.);
#3319=VECTOR('',#12302,1000.);
#3320=VECTOR('',#12303,1000.);
#3321=VECTOR('',#12306,1000.);
#3322=VECTOR('',#12307,1000.);
#3323=VECTOR('',#12310,1000.);
#3324=VECTOR('',#12313,1000.);
#3325=VECTOR('',#12316,1000.);
#3326=VECTOR('',#12319,1000.);
#3327=VECTOR('',#12320,1000.);
#3328=VECTOR('',#12323,1000.);
#3329=VECTOR('',#12324,1000.);
#3330=VECTOR('',#12327,1000.);
#3331=VECTOR('',#12328,1000.);
#3332=VECTOR('',#12331,1000.);
#3333=VECTOR('',#12334,1000.);
#3334=VECTOR('',#12357,1000.);
#3335=VECTOR('',#12358,1000.);
#3336=VECTOR('',#12461,1000.);
#3337=VECTOR('',#12462,1000.);
#3338=VECTOR('',#12465,1000.);
#3339=VECTOR('',#12466,1000.);
#3340=VECTOR('',#12469,1000.);
#3341=VECTOR('',#12470,1000.);
#3342=VECTOR('',#12473,1000.);
#3343=VECTOR('',#12474,1000.);
#3344=VECTOR('',#12477,1000.);
#3345=VECTOR('',#12478,1000.);
#3346=VECTOR('',#12481,1000.);
#3347=VECTOR('',#12482,1000.);
#3348=VECTOR('',#12485,1000.);
#3349=VECTOR('',#12486,1000.);
#3350=VECTOR('',#12489,1000.);
#3351=VECTOR('',#12490,1000.);
#3352=VECTOR('',#12493,1000.);
#3353=VECTOR('',#12494,1000.);
#3354=VECTOR('',#12497,1000.);
#3355=VECTOR('',#12498,1000.);
#3356=VECTOR('',#12503,10.922);
#3357=VECTOR('',#12514,1000.);
#3358=VECTOR('',#12517,1000.);
#3359=VECTOR('',#12522,3.24485);
#3360=VECTOR('',#12529,4.03225);
#3361=VECTOR('',#12534,1000.);
#3362=VECTOR('',#12535,1000.);
#3363=VECTOR('',#12536,1000.);
#3364=VECTOR('',#12537,1000.);
#3365=VECTOR('',#12538,1000.);
#3366=VECTOR('',#12539,1000.);
#3367=VECTOR('',#12542,1000.);
#3368=VECTOR('',#12543,1000.);
#3369=VECTOR('',#12546,1000.);
#3370=VECTOR('',#12549,1000.);
#3371=VECTOR('',#12550,1000.);
#3372=VECTOR('',#12551,1000.);
#3373=VECTOR('',#12554,1000.);
#3374=VECTOR('',#12557,1000.);
#3375=VECTOR('',#12572,1000.);
#3376=VECTOR('',#12573,1000.);
#3377=VECTOR('',#12576,1000.);
#3378=VECTOR('',#12579,1000.);
#3379=VECTOR('',#12582,1000.);
#3380=VECTOR('',#12583,1000.);
#3381=VECTOR('',#12586,1000.);
#3382=VECTOR('',#12587,1000.);
#3383=VECTOR('',#12596,1000.);
#3384=VECTOR('',#12597,1000.);
#3385=VECTOR('',#12604,1000.);
#3386=VECTOR('',#12605,1000.);
#3387=VECTOR('',#12612,1000.);
#3388=VECTOR('',#12613,1000.);
#3389=VECTOR('',#12616,1000.);
#3390=VECTOR('',#12617,1000.);
#3391=VECTOR('',#12620,1000.);
#3392=VECTOR('',#12621,1000.);
#3393=VECTOR('',#12624,1000.);
#3394=VECTOR('',#12629,1000.);
#3395=VECTOR('',#12638,1000.);
#3396=VECTOR('',#12639,1000.);
#3397=VECTOR('',#12650,1000.);
#3398=VECTOR('',#12651,1000.);
#3399=VECTOR('',#12654,1000.);
#3400=VECTOR('',#12655,1000.);
#3401=VECTOR('',#12658,1000.);
#3402=VECTOR('',#12663,1000.);
#3403=VECTOR('',#12698,1000.);
#3404=VECTOR('',#12699,1000.);
#3405=VECTOR('',#12702,1000.);
#3406=VECTOR('',#12703,1000.);
#3407=VECTOR('',#12706,1000.);
#3408=VECTOR('',#12707,1000.);
#3409=VECTOR('',#12736,1000.);
#3410=VECTOR('',#12743,1000.);
#3411=VECTOR('',#12746,1000.);
#3412=VECTOR('',#12751,1000.);
#3413=VECTOR('',#12754,1000.);
#3414=VECTOR('',#12759,1000.);
#3415=VECTOR('',#12766,1000.);
#3416=VECTOR('',#12767,1000.);
#3417=VECTOR('',#12770,1000.);
#3418=VECTOR('',#12771,1000.);
#3419=VECTOR('',#12774,1000.);
#3420=VECTOR('',#12775,1000.);
#3421=VECTOR('',#12778,1000.);
#3422=VECTOR('',#12783,1000.);
#3423=VECTOR('',#12792,1000.);
#3424=VECTOR('',#12793,1000.);
#3425=VECTOR('',#12804,1000.);
#3426=VECTOR('',#12805,1000.);
#3427=VECTOR('',#12812,1000.);
#3428=VECTOR('',#12813,1000.);
#3429=VECTOR('',#12824,1000.);
#3430=VECTOR('',#12829,1000.);
#3431=VECTOR('',#12844,1000.);
#3432=VECTOR('',#12845,1000.);
#3433=VECTOR('',#12848,1000.);
#3434=VECTOR('',#12849,1000.);
#3435=VECTOR('',#12852,1000.);
#3436=VECTOR('',#12853,1000.);
#3437=VECTOR('',#12856,1000.);
#3438=VECTOR('',#12861,1000.);
#3439=VECTOR('',#12870,1000.);
#3440=VECTOR('',#12871,1000.);
#3441=VECTOR('',#12878,1000.);
#3442=VECTOR('',#12879,1000.);
#3443=VECTOR('',#12884,1000.);
#3444=VECTOR('',#12893,1000.);
#3445=VECTOR('',#12908,1000.);
#3446=VECTOR('',#12909,1000.);
#3447=VECTOR('',#12914,1000.);
#3448=VECTOR('',#12919,1000.);
#3449=VECTOR('',#12934,1000.);
#3450=VECTOR('',#12937,1000.);
#3451=VECTOR('',#12944,1000.);
#3452=VECTOR('',#12947,1000.);
#3453=VECTOR('',#12954,1000.);
#3454=VECTOR('',#12957,1000.);
#3455=VECTOR('',#12978,1000.);
#3456=VECTOR('',#12981,1000.);
#3457=VECTOR('',#12982,1000.);
#3458=VECTOR('',#12985,1000.);
#3459=VECTOR('',#12986,1000.);
#3460=VECTOR('',#12989,1000.);
#3461=VECTOR('',#13014,3.9243);
#3462=VECTOR('',#13027,3.175);
#3463=VECTOR('',#13032,3.175);
#3464=VECTOR('',#13063,1000.);
#3465=VECTOR('',#13064,1000.);
#3466=VECTOR('',#13065,1000.);
#3467=VECTOR('',#13068,1000.);
#3468=VECTOR('',#13069,1000.);
#3469=VECTOR('',#13072,1000.);
#3470=VECTOR('',#13073,1000.);
#3471=VECTOR('',#13076,1000.);
#3472=VECTOR('',#13077,1000.);
#3473=VECTOR('',#13080,1000.);
#3474=VECTOR('',#13081,1000.);
#3475=VECTOR('',#13084,1000.);
#3476=VECTOR('',#13097,5.6515);
#3477=VECTOR('',#13116,9.59611131114252);
#3478=VECTOR('',#13121,15.3208607241417);
#3479=VECTOR('',#13134,19.05);
#3480=VECTOR('',#13165,8.56864389726312);
#3481=VECTOR('',#13194,5.4991);
#3482=VECTOR('',#13211,3.175);
#3483=VECTOR('',#13218,2.48793);
#3484=VECTOR('',#13223,2.48793);
#3485=VECTOR('',#13254,1000.);
#3486=VECTOR('',#13255,1000.);
#3487=VECTOR('',#13256,1000.);
#3488=VECTOR('',#13257,1000.);
#3489=VECTOR('',#13260,1000.);
#3490=VECTOR('',#13261,1000.);
#3491=VECTOR('',#13262,1000.);
#3492=VECTOR('',#13265,1000.);
#3493=VECTOR('',#13266,1000.);
#3494=VECTOR('',#13267,1000.);
#3495=VECTOR('',#13270,1000.);
#3496=VECTOR('',#13271,1000.);
#3497=VECTOR('',#13272,1000.);
#3498=VECTOR('',#13275,1000.);
#3499=VECTOR('',#13276,1000.);
#3500=VECTOR('',#13277,1000.);
#3501=VECTOR('',#13280,1000.);
#3502=VECTOR('',#13281,1000.);
#3503=VECTOR('',#13314,5.30225);
#3504=VECTOR('',#13315,1000.);
#3505=VECTOR('',#13318,1000.);
#3506=VECTOR('',#13323,4.03225);
#3507=VECTOR('',#13330,5.55625);
#3508=VECTOR('',#13343,3.5687);
#3509=VECTOR('',#13348,5.55625);
#3510=VECTOR('',#13361,9.525);
#3511=VECTOR('',#13366,9.525);
#3512=VECTOR('',#13381,5.4991);
#3513=VECTOR('',#13386,5.4991);
#3514=VECTOR('',#13389,1000.);
#3515=VECTOR('',#13392,1000.);
#3516=VECTOR('',#13427,5.6388);
#3517=VECTOR('',#13442,9.49667180024818);
#3518=VECTOR('',#13475,11.0475234888716);
#3519=VECTOR('',#13486,1000.);
#3520=VECTOR('',#13487,1000.);
#3521=VECTOR('',#13488,1000.);
#3522=VECTOR('',#13489,1000.);
#3523=VECTOR('',#13492,1000.);
#3524=VECTOR('',#13493,1000.);
#3525=VECTOR('',#13494,1000.);
#3526=VECTOR('',#13497,1000.);
#3527=VECTOR('',#13498,1000.);
#3528=VECTOR('',#13499,1000.);
#3529=VECTOR('',#13502,1000.);
#3530=VECTOR('',#13503,1000.);
#3531=VECTOR('',#13504,1000.);
#3532=VECTOR('',#13507,1000.);
#3533=VECTOR('',#13508,1000.);
#3534=VECTOR('',#13509,1000.);
#3535=VECTOR('',#13512,1000.);
#3536=VECTOR('',#13513,1000.);
#3537=VECTOR('',#13514,1000.);
#3538=VECTOR('',#13517,1000.);
#3539=VECTOR('',#13518,1000.);
#3540=VECTOR('',#13519,1000.);
#3541=VECTOR('',#13522,1000.);
#3542=VECTOR('',#13523,1000.);
#3543=VECTOR('',#13538,12.7);
#3544=VECTOR('',#13545,36.9094469866104);
#3545=VECTOR('',#13552,39.751);
#3546=VECTOR('',#13567,45.30725);
#3547=VECTOR('',#13578,39.751);
#3548=VECTOR('',#13585,37.465);
#3549=VECTOR('',#13592,14.1695751798421);
#3550=VECTOR('',#13599,7.7216);
#3551=VECTOR('',#13624,39.751);
#3552=VECTOR('',#13637,45.30725);
#3553=VECTOR('',#13650,39.751);
#3554=VECTOR('',#13667,42.8625);
#3555=VECTOR('',#13682,50.4073015581831);
#3556=VECTOR('',#13687,50.8);
#3557=VECTOR('',#13698,48.9603369133721);
#3558=VECTOR('',#13721,4.0386);
#3559=VECTOR('',#13728,5.55625);
#3560=VECTOR('',#13741,6.0325);
#3561=VECTOR('',#13748,5.6515);
#3562=VECTOR('',#13753,5.6515);
#3563=VECTOR('',#13760,7.6835);
#3564=CIRCLE('',#9752,6.00000000000002);
#3565=CIRCLE('',#9753,6.00000000000002);
#3566=CIRCLE('',#9755,6.00000000000001);
#3567=CIRCLE('',#9756,6.00000000000001);
#3568=CIRCLE('',#9758,6.00000000000002);
#3569=CIRCLE('',#9759,6.00000000000002);
#3570=CIRCLE('',#9761,6.00000000000001);
#3571=CIRCLE('',#9762,6.00000000000001);
#3572=CIRCLE('',#9764,6.34999999999999);
#3573=CIRCLE('',#9765,6.34999999999999);
#3574=CIRCLE('',#9767,6.35000000000122);
#3575=CIRCLE('',#9768,6.35000000000122);
#3576=CIRCLE('',#9770,6.35000000000122);
#3577=CIRCLE('',#9771,6.35000000000122);
#3578=CIRCLE('',#9773,6.46290152238551);
#3579=CIRCLE('',#9774,6.4629015223855);
#3580=CIRCLE('',#9776,6.4629015223855);
#3581=CIRCLE('',#9777,6.4629015223855);
#3582=CIRCLE('',#9779,6.34999999999994);
#3583=CIRCLE('',#9780,6.34999999999994);
#3584=CIRCLE('',#9782,6.34999999999994);
#3585=CIRCLE('',#9783,6.34999999999994);
#3586=CIRCLE('',#9785,4.);
#3587=CIRCLE('',#9787,4.);
#3588=CIRCLE('',#9791,4.);
#3589=CIRCLE('',#9793,4.);
#3590=CIRCLE('',#9795,4.);
#3591=CIRCLE('',#9796,1.);
#3592=CIRCLE('',#9799,4.);
#3593=CIRCLE('',#9800,1.);
#3594=CIRCLE('',#9803,4.);
#3595=CIRCLE('',#9804,1.);
#3596=CIRCLE('',#9807,4.);
#3597=CIRCLE('',#9808,1.);
#3598=CIRCLE('',#9811,4.);
#3599=CIRCLE('',#9812,1.);
#3600=CIRCLE('',#9814,4.);
#3601=CIRCLE('',#9815,1.);
#3602=CIRCLE('',#9818,4.);
#3603=CIRCLE('',#9819,1.);
#3604=CIRCLE('',#9822,4.);
#3605=CIRCLE('',#9823,1.);
#3606=CIRCLE('',#9825,4.);
#3607=CIRCLE('',#9826,1.);
#3608=CIRCLE('',#9829,4.);
#3609=CIRCLE('',#9830,1.);
#3610=CIRCLE('',#9857,4.);
#3611=CIRCLE('',#9858,1.);
#3612=CIRCLE('',#9860,4.);
#3613=CIRCLE('',#9861,1.);
#3614=CIRCLE('',#9872,1.);
#3615=CIRCLE('',#9873,4.);
#3616=CIRCLE('',#9875,4.);
#3617=CIRCLE('',#9876,1.);
#3618=CIRCLE('',#9888,6.00000000000001);
#3619=CIRCLE('',#9889,6.00000000000001);
#3620=CIRCLE('',#9891,6.00000000000002);
#3621=CIRCLE('',#9892,6.00000000000001);
#3622=CIRCLE('',#9894,6.00000000000001);
#3623=CIRCLE('',#9895,6.00000000000001);
#3624=CIRCLE('',#9897,6.00000000000001);
#3625=CIRCLE('',#9898,6.00000000000002);
#3626=CIRCLE('',#9900,6.34999999999994);
#3627=CIRCLE('',#9901,6.34999999999994);
#3628=CIRCLE('',#9903,6.34999999999994);
#3629=CIRCLE('',#9904,6.34999999999997);
#3630=CIRCLE('',#9906,6.34999999999995);
#3631=CIRCLE('',#9907,6.34999999999995);
#3632=CIRCLE('',#9909,6.34999999999997);
#3633=CIRCLE('',#9910,6.34999999999997);
#3634=CIRCLE('',#9912,4.);
#3635=CIRCLE('',#9914,4.);
#3636=CIRCLE('',#9918,4.);
#3637=CIRCLE('',#9920,4.);
#3638=CIRCLE('',#9922,4.);
#3639=CIRCLE('',#9923,1.);
#3640=CIRCLE('',#9926,4.);
#3641=CIRCLE('',#9927,1.);
#3642=CIRCLE('',#9930,4.);
#3643=CIRCLE('',#9931,1.);
#3644=CIRCLE('',#9933,4.);
#3645=CIRCLE('',#9934,1.);
#3646=CIRCLE('',#9937,4.);
#3647=CIRCLE('',#9938,1.);
#3648=CIRCLE('',#9941,4.);
#3649=CIRCLE('',#9942,1.);
#3650=CIRCLE('',#9944,4.);
#3651=CIRCLE('',#9945,1.);
#3652=CIRCLE('',#9948,4.);
#3653=CIRCLE('',#9949,1.);
#3654=CIRCLE('',#9952,4.);
#3655=CIRCLE('',#9953,1.);
#3656=CIRCLE('',#9956,4.);
#3657=CIRCLE('',#9957,1.);
#3658=CIRCLE('',#9984,4.);
#3659=CIRCLE('',#9985,1.);
#3660=CIRCLE('',#9987,4.);
#3661=CIRCLE('',#9988,1.);
#3662=CIRCLE('',#9999,1.);
#3663=CIRCLE('',#10000,4.);
#3664=CIRCLE('',#10002,4.);
#3665=CIRCLE('',#10003,1.);
#3666=CIRCLE('',#10015,6.34999999871023);
#3667=CIRCLE('',#10016,6.34999999871023);
#3668=CIRCLE('',#10018,6.34999999871025);
#3669=CIRCLE('',#10019,6.34999999871025);
#3670=CIRCLE('',#10021,6.34999999999997);
#3671=CIRCLE('',#10022,6.34999999999997);
#3672=CIRCLE('',#10024,6.98053323984749);
#3673=CIRCLE('',#10025,6.98053323984749);
#3674=CIRCLE('',#10027,6.35);
#3675=CIRCLE('',#10028,6.35);
#3676=CIRCLE('',#10030,6.34999999999999);
#3677=CIRCLE('',#10031,6.34999999999999);
#3678=CIRCLE('',#10033,6.35);
#3679=CIRCLE('',#10034,6.35);
#3680=CIRCLE('',#10036,6.35);
#3681=CIRCLE('',#10037,6.35);
#3682=CIRCLE('',#10040,1.);
#3683=CIRCLE('',#10041,4.);
#3684=CIRCLE('',#10044,1.);
#3685=CIRCLE('',#10045,4.);
#3686=CIRCLE('',#10048,1.);
#3687=CIRCLE('',#10049,4.);
#3688=CIRCLE('',#10052,1.);
#3689=CIRCLE('',#10053,4.);
#3690=CIRCLE('',#10082,7.11098481470124);
#3691=CIRCLE('',#10083,7.11098481470124);
#3692=CIRCLE('',#10085,6.34999999871023);
#3693=CIRCLE('',#10086,6.34999999871023);
#3694=CIRCLE('',#10088,6.34999999999997);
#3695=CIRCLE('',#10089,6.34999999999997);
#3696=CIRCLE('',#10091,6.98053323984749);
#3697=CIRCLE('',#10092,6.98053323984749);
#3698=CIRCLE('',#10094,6.35);
#3699=CIRCLE('',#10095,6.35);
#3700=CIRCLE('',#10097,6.34999999999999);
#3701=CIRCLE('',#10098,6.34999999999999);
#3702=CIRCLE('',#10100,6.35);
#3703=CIRCLE('',#10101,6.35);
#3704=CIRCLE('',#10103,6.35);
#3705=CIRCLE('',#10104,6.35);
#3706=CIRCLE('',#10107,4.);
#3707=CIRCLE('',#10108,1.);
#3708=CIRCLE('',#10111,4.);
#3709=CIRCLE('',#10112,1.);
#3710=CIRCLE('',#10115,4.);
#3711=CIRCLE('',#10116,1.);
#3712=CIRCLE('',#10119,4.);
#3713=CIRCLE('',#10120,1.);
#3714=CIRCLE('',#10149,6.34999999999999);
#3715=CIRCLE('',#10150,6.34999999999999);
#3716=CIRCLE('',#10152,6.34999999999999);
#3717=CIRCLE('',#10153,6.34999999999999);
#3718=CIRCLE('',#10155,6.35);
#3719=CIRCLE('',#10156,6.35);
#3720=CIRCLE('',#10158,1.);
#3721=CIRCLE('',#10159,5.7625);
#3722=CIRCLE('',#10162,1.);
#3723=CIRCLE('',#10163,5.7625);
#3724=CIRCLE('',#10166,5.7625);
#3725=CIRCLE('',#10167,1.);
#3726=CIRCLE('',#10170,5.7625);
#3727=CIRCLE('',#10171,1.);
#3728=CIRCLE('',#10174,5.7625);
#3729=CIRCLE('',#10175,1.);
#3730=CIRCLE('',#10178,5.7625);
#3731=CIRCLE('',#10179,1.);
#3732=CIRCLE('',#10186,1.);
#3733=CIRCLE('',#10187,1.);
#3734=CIRCLE('',#10204,5.7625);
#3735=CIRCLE('',#10205,5.7625);
#3736=CIRCLE('',#10213,4.);
#3737=CIRCLE('',#10214,1.);
#3738=CIRCLE('',#10217,4.);
#3739=CIRCLE('',#10218,1.);
#3740=CIRCLE('',#10221,4.);
#3741=CIRCLE('',#10222,1.);
#3742=CIRCLE('',#10225,4.);
#3743=CIRCLE('',#10226,1.);
#3744=CIRCLE('',#10246,23.749);
#3745=CIRCLE('',#10247,26.924);
#3746=CIRCLE('',#10251,26.924);
#3747=CIRCLE('',#10253,26.924);
#3748=CIRCLE('',#10255,26.924);
#3749=CIRCLE('',#10257,26.924);
#3750=CIRCLE('',#10259,26.924);
#3751=CIRCLE('',#10261,26.924);
#3752=CIRCLE('',#10262,226.762223222856);
#3753=CIRCLE('',#10263,26.924);
#3754=CIRCLE('',#10265,26.924);
#3755=CIRCLE('',#10267,26.924);
#3756=CIRCLE('',#10268,26.924);
#3757=CIRCLE('',#10269,212.717904512561);
#3758=CIRCLE('',#10270,26.924);
#3759=CIRCLE('',#10272,26.924);
#3760=CIRCLE('',#10273,218.610255921951);
#3761=CIRCLE('',#10274,26.924);
#3762=CIRCLE('',#10276,26.924);
#3763=CIRCLE('',#10277,220.587567903402);
#3764=CIRCLE('',#10278,26.924);
#3765=CIRCLE('',#10280,228.291094002382);
#3766=CIRCLE('',#10281,26.924);
#3767=CIRCLE('',#10282,221.635215639641);
#3768=CIRCLE('',#10283,26.924);
#3769=CIRCLE('',#10284,230.154148290915);
#3770=CIRCLE('',#10285,26.924);
#3771=CIRCLE('',#10287,26.924);
#3772=CIRCLE('',#10289,26.924);
#3773=CIRCLE('',#10291,27.4531089883189);
#3774=CIRCLE('',#10292,228.33704976361);
#3775=CIRCLE('',#10293,26.924);
#3776=CIRCLE('',#10295,26.924);
#3777=CIRCLE('',#10297,26.924);
#3778=CIRCLE('',#10299,27.4552594201478);
#3779=CIRCLE('',#10311,10.922);
#3780=CIRCLE('',#10312,10.922);
#3781=CIRCLE('',#10314,21.209);
#3782=CIRCLE('',#10315,24.384);
#3783=CIRCLE('',#10319,3.24485);
#3784=CIRCLE('',#10320,3.24485);
#3785=CIRCLE('',#10322,4.03225);
#3786=CIRCLE('',#10323,4.03225);
#3787=CIRCLE('',#10331,11.1252);
#3788=CIRCLE('',#10332,11.1252);
#3789=CIRCLE('',#10334,11.1252);
#3790=CIRCLE('',#10335,11.1252);
#3791=CIRCLE('',#10346,26.0773333333334);
#3792=CIRCLE('',#10356,26.0773333333334);
#3793=CIRCLE('',#10361,26.0773333333334);
#3794=CIRCLE('',#10369,26.0773333333334);
#3795=CIRCLE('',#10373,26.0773333333334);
#3796=CIRCLE('',#10375,221.040072583319);
#3797=CIRCLE('',#10377,26.5896319406819);
#3798=CIRCLE('',#10379,26.0773333333334);
#3799=CIRCLE('',#10381,222.916006880037);
#3800=CIRCLE('',#10383,26.5918522144337);
#3801=CIRCLE('',#10389,214.124017737833);
#3802=CIRCLE('',#10391,26.0773333333334);
#3803=CIRCLE('',#10393,220.992609647167);
#3804=CIRCLE('',#10395,26.0773333333334);
#3805=CIRCLE('',#10397,26.0773333333334);
#3806=CIRCLE('',#10398,217.504636483604);
#3807=CIRCLE('',#10399,26.0773333333334);
#3808=CIRCLE('',#10400,218.812383348363);
#3809=CIRCLE('',#10402,26.924);
#3810=CIRCLE('',#10404,224.911644303999);
#3811=CIRCLE('',#10407,26.924);
#3812=CIRCLE('',#10410,226.178827974078);
#3813=CIRCLE('',#10417,213.043442242318);
#3814=CIRCLE('',#10419,26.0773333333334);
#3815=CIRCLE('',#10424,26.0773333333334);
#3816=CIRCLE('',#10426,204.92922099147);
#3817=CIRCLE('',#10429,26.0773333333334);
#3818=CIRCLE('',#10434,26.0773333333334);
#3819=CIRCLE('',#10438,26.0773333333334);
#3820=CIRCLE('',#10440,211.00405738226);
#3821=CIRCLE('',#10442,26.0773333333334);
#3822=CIRCLE('',#10450,26.0773333333334);
#3823=CIRCLE('',#10455,26.0773333333334);
#3824=CIRCLE('',#10459,26.0773333333334);
#3825=CIRCLE('',#10465,26.0773333333334);
#3826=CIRCLE('',#10467,26.0773333333334);
#3827=CIRCLE('',#10472,26.0773333333334);
#3828=CIRCLE('',#10474,222.811288236089);
#3829=CIRCLE('',#10476,26.0773333333334);
#3830=CIRCLE('',#10479,216.62089092034);
#3831=CIRCLE('',#10480,224.055220201137);
#3832=CIRCLE('',#10483,26.0773333333334);
#3833=CIRCLE('',#10484,26.924);
#3834=CIRCLE('',#10487,215.027560828879);
#3835=CIRCLE('',#10488,222.510963061353);
#3836=CIRCLE('',#10491,26.0773333333334);
#3837=CIRCLE('',#10492,26.924);
#3838=CIRCLE('',#10495,219.414478611741);
#3839=CIRCLE('',#10496,26.0773333333334);
#3840=CIRCLE('',#10498,26.0773333333334);
#3841=CIRCLE('',#10510,3.9243);
#3842=CIRCLE('',#10511,0.508);
#3843=CIRCLE('',#10512,4.4323);
#3844=CIRCLE('',#10514,3.9243);
#3845=CIRCLE('',#10516,3.4163);
#3846=CIRCLE('',#10517,0.507999999999992);
#3847=CIRCLE('',#10519,3.175);
#3848=CIRCLE('',#10520,3.175);
#3849=CIRCLE('',#10521,3.175);
#3850=CIRCLE('',#10523,2.1844);
#3851=CIRCLE('',#10525,5.588);
#3852=CIRCLE('',#10527,5.588);
#3853=CIRCLE('',#10528,5.588);
#3854=CIRCLE('',#10529,5.588);
#3855=CIRCLE('',#10530,5.588);
#3856=CIRCLE('',#10531,5.588);
#3857=CIRCLE('',#10548,5.6515);
#3858=CIRCLE('',#10549,5.6515);
#3859=CIRCLE('',#10551,8.52204264558423);
#3860=CIRCLE('',#10552,1.143);
#3861=CIRCLE('',#10553,9.59611131114252);
#3862=CIRCLE('',#10554,9.59611131114252);
#3863=CIRCLE('',#10556,10.3807974512434);
#3864=CIRCLE('',#10557,10.3807974512434);
#3865=CIRCLE('',#10559,16.5763055377746);
#3866=CIRCLE('',#10560,17.5196750989302);
#3867=CIRCLE('',#10562,1.5748);
#3868=CIRCLE('',#10563,18.5282252464232);
#3869=CIRCLE('',#10565,19.05);
#3870=CIRCLE('',#10566,19.05);
#3871=CIRCLE('',#10568,18.4629769854638);
#3872=CIRCLE('',#10569,0.7874);
#3873=CIRCLE('',#10570,17.7942315496296);
#3874=CIRCLE('',#10572,5.1308);
#3875=CIRCLE('',#10573,13.4366);
#3876=CIRCLE('',#10575,13.3900187959915);
#3877=CIRCLE('',#10576,5.1308);
#3878=CIRCLE('',#10577,8.56864389726312);
#3879=CIRCLE('',#10578,8.56864389726312);
#3880=CIRCLE('',#10580,7.6397314493846);
#3881=CIRCLE('',#10581,7.6397314493846);
#3882=CIRCLE('',#10583,1.143);
#3883=CIRCLE('',#10584,6.5656627838263);
#3884=CIRCLE('',#10586,3.3528);
#3885=CIRCLE('',#10594,5.4991);
#3886=CIRCLE('',#10595,5.4991);
#3887=CIRCLE('',#10596,5.4991);
#3888=CIRCLE('',#10597,5.4991);
#3889=CIRCLE('',#10598,5.4991);
#3890=CIRCLE('',#10599,5.4991);
#3891=CIRCLE('',#10600,5.4991);
#3892=CIRCLE('',#10602,2.48793);
#3893=CIRCLE('',#10603,3.175);
#3894=CIRCLE('',#10604,2.48793);
#3895=CIRCLE('',#10606,2.48793);
#3896=CIRCLE('',#10608,3.175);
#3897=CIRCLE('',#10610,5.4991);
#3898=CIRCLE('',#10612,5.4991);
#3899=CIRCLE('',#10613,5.4991);
#3900=CIRCLE('',#10614,5.4991);
#3901=CIRCLE('',#10615,5.4991);
#3902=CIRCLE('',#10616,5.4991);
#3903=CIRCLE('',#10637,0.762);
#3904=CIRCLE('',#10638,5.32701449118557);
#3905=CIRCLE('',#10639,5.32701449118557);
#3906=CIRCLE('',#10640,0.762);
#3907=CIRCLE('',#10641,5.10079889800413);
#3908=CIRCLE('',#10643,5.55625);
#3909=CIRCLE('',#10644,5.30225);
#3910=CIRCLE('',#10646,5.55625);
#3911=CIRCLE('',#10647,4.03225);
#3912=CIRCLE('',#10649,5.55625);
#3913=CIRCLE('',#10651,3.5687);
#3914=CIRCLE('',#10652,0.3175);
#3915=CIRCLE('',#10653,3.8862);
#3916=CIRCLE('',#10655,3.5687);
#3917=CIRCLE('',#10657,5.55625);
#3918=CIRCLE('',#10659,6.06425);
#3919=CIRCLE('',#10660,0.508);
#3920=CIRCLE('',#10662,9.525);
#3921=CIRCLE('',#10663,9.525);
#3922=CIRCLE('',#10664,9.525);
#3923=CIRCLE('',#10666,8.6995);
#3924=CIRCLE('',#10668,5.4991);
#3925=CIRCLE('',#10669,0.508);
#3926=CIRCLE('',#10670,6.0071);
#3927=CIRCLE('',#10672,5.4991);
#3928=CIRCLE('',#10674,8.6995);
#3929=CIRCLE('',#10685,16.0314200400514);
#3930=CIRCLE('',#10686,2.413127);
#3931=CIRCLE('',#10687,17.2933799599486);
#3932=CIRCLE('',#10689,14.0623779989364);
#3933=CIRCLE('',#10690,14.0623779989364);
#3934=CIRCLE('',#10691,3.429);
#3935=CIRCLE('',#10693,5.6388);
#3936=CIRCLE('',#10694,5.6388);
#3937=CIRCLE('',#10696,8.89);
#3938=CIRCLE('',#10697,0.8001);
#3939=CIRCLE('',#10698,9.49667180024818);
#3940=CIRCLE('',#10699,9.49667180024818);
#3941=CIRCLE('',#10702,3.429);
#3942=CIRCLE('',#10703,19.5325471456964);
#3943=CIRCLE('',#10705,3.302);
#3944=CIRCLE('',#10706,22.296392545256);
#3945=CIRCLE('',#10708,23.1013);
#3946=CIRCLE('',#10709,3.302);
#3947=CIRCLE('',#10710,21.3609133903113);
#3948=CIRCLE('',#10712,6.477);
#3949=CIRCLE('',#10713,11.0475234888716);
#3950=CIRCLE('',#10714,11.0475234888716);
#3951=CIRCLE('',#10716,9.4771047851023);
#3952=CIRCLE('',#10717,9.4771047851023);
#3953=CIRCLE('',#10719,1.6002);
#3954=CIRCLE('',#10720,8.0899);
#3955=CIRCLE('',#10735,14.1695751798421);
#3956=CIRCLE('',#10736,12.7);
#3957=CIRCLE('',#10738,36.9094469866104);
#3958=CIRCLE('',#10739,37.465);
#3959=CIRCLE('',#10741,39.751);
#3960=CIRCLE('',#10742,39.751);
#3961=CIRCLE('',#10744,45.30725);
#3962=CIRCLE('',#10745,3.302);
#3963=CIRCLE('',#10746,42.00525);
#3964=CIRCLE('',#10748,45.30725);
#3965=CIRCLE('',#10750,42.00525);
#3966=CIRCLE('',#10751,3.302);
#3967=CIRCLE('',#10753,39.751);
#3968=CIRCLE('',#10754,39.751);
#3969=CIRCLE('',#10756,36.9094469866104);
#3970=CIRCLE('',#10757,37.465);
#3971=CIRCLE('',#10759,14.1695751798421);
#3972=CIRCLE('',#10760,12.7);
#3973=CIRCLE('',#10762,7.7216);
#3974=CIRCLE('',#10763,7.7216);
#3975=CIRCLE('',#10774,39.751);
#3976=CIRCLE('',#10775,39.751);
#3977=CIRCLE('',#10777,42.00525);
#3978=CIRCLE('',#10778,3.302);
#3979=CIRCLE('',#10779,45.30725);
#3980=CIRCLE('',#10781,45.30725);
#3981=CIRCLE('',#10783,3.302);
#3982=CIRCLE('',#10784,42.00525);
#3983=CIRCLE('',#10786,39.751);
#3984=CIRCLE('',#10787,39.751);
#3985=CIRCLE('',#10789,41.275);
#3986=CIRCLE('',#10790,1.5875);
#3987=CIRCLE('',#10791,42.8625);
#3988=CIRCLE('',#10792,42.8625);
#3989=CIRCLE('',#10794,48.9603369133721);
#3990=CIRCLE('',#10795,48.9603369133721);
#3991=CIRCLE('',#10797,1.5875);
#3992=CIRCLE('',#10798,50.4073015581831);
#3993=CIRCLE('',#10799,50.4073015581831);
#3994=CIRCLE('',#10801,50.8);
#3995=CIRCLE('',#10802,50.8);
#3996=CIRCLE('',#10804,50.4073015581831);
#3997=CIRCLE('',#10806,1.5875);
#3998=CIRCLE('',#10807,48.9603369133721);
#3999=CIRCLE('',#10809,42.8625);
#4000=CIRCLE('',#10811,1.5875);
#4001=CIRCLE('',#10812,41.275);
#4002=CIRCLE('',#10819,4.0386);
#4003=CIRCLE('',#10820,4.0386);
#4004=CIRCLE('',#10822,5.55625);
#4005=CIRCLE('',#10823,5.55625);
#4006=CIRCLE('',#10828,5.6515);
#4007=CIRCLE('',#10829,6.0325);
#4008=CIRCLE('',#10830,5.6515);
#4009=CIRCLE('',#10832,5.6515);
#4010=CIRCLE('',#10834,6.0325);
#4011=CIRCLE('',#10836,7.6835);
#4012=CIRCLE('',#10837,7.6835);
#4013=VERTEX_POINT('',#13812);
#4014=VERTEX_POINT('',#13814);
#4015=VERTEX_POINT('',#13818);
#4016=VERTEX_POINT('',#13820);
#4017=VERTEX_POINT('',#13824);
#4018=VERTEX_POINT('',#13826);
#4019=VERTEX_POINT('',#13830);
#4020=VERTEX_POINT('',#13832);
#4021=VERTEX_POINT('',#13836);
#4022=VERTEX_POINT('',#13838);
#4023=VERTEX_POINT('',#13842);
#4024=VERTEX_POINT('',#13844);
#4025=VERTEX_POINT('',#13848);
#4026=VERTEX_POINT('',#13850);
#4027=VERTEX_POINT('',#13854);
#4028=VERTEX_POINT('',#13856);
#4029=VERTEX_POINT('',#13860);
#4030=VERTEX_POINT('',#13862);
#4031=VERTEX_POINT('',#13866);
#4032=VERTEX_POINT('',#13868);
#4033=VERTEX_POINT('',#13872);
#4034=VERTEX_POINT('',#13874);
#4035=VERTEX_POINT('',#13878);
#4036=VERTEX_POINT('',#13879);
#4037=VERTEX_POINT('',#13881);
#4038=VERTEX_POINT('',#13883);
#4039=VERTEX_POINT('',#13887);
#4040=VERTEX_POINT('',#13888);
#4041=VERTEX_POINT('',#13890);
#4042=VERTEX_POINT('',#13892);
#4043=VERTEX_POINT('',#13896);
#4044=VERTEX_POINT('',#13899);
#4045=VERTEX_POINT('',#13903);
#4046=VERTEX_POINT('',#13904);
#4047=VERTEX_POINT('',#13906);
#4048=VERTEX_POINT('',#13908);
#4049=VERTEX_POINT('',#13912);
#4050=VERTEX_POINT('',#13913);
#4051=VERTEX_POINT('',#13916);
#4052=VERTEX_POINT('',#13920);
#4053=VERTEX_POINT('',#13922);
#4054=VERTEX_POINT('',#13924);
#4055=VERTEX_POINT('',#13928);
#4056=VERTEX_POINT('',#13929);
#4057=VERTEX_POINT('',#13931);
#4058=VERTEX_POINT('',#13933);
#4059=VERTEX_POINT('',#13937);
#4060=VERTEX_POINT('',#13939);
#4061=VERTEX_POINT('',#13943);
#4062=VERTEX_POINT('',#13944);
#4063=VERTEX_POINT('',#13946);
#4064=VERTEX_POINT('',#13948);
#4065=VERTEX_POINT('',#13952);
#4066=VERTEX_POINT('',#13954);
#4067=VERTEX_POINT('',#13958);
#4068=VERTEX_POINT('',#13959);
#4069=VERTEX_POINT('',#13964);
#4070=VERTEX_POINT('',#13966);
#4071=VERTEX_POINT('',#13970);
#4072=VERTEX_POINT('',#13971);
#4073=VERTEX_POINT('',#13973);
#4074=VERTEX_POINT('',#13975);
#4075=VERTEX_POINT('',#13985);
#4076=VERTEX_POINT('',#13986);
#4077=VERTEX_POINT('',#13994);
#4078=VERTEX_POINT('',#13995);
#4079=VERTEX_POINT('',#14000);
#4080=VERTEX_POINT('',#14002);
#4081=VERTEX_POINT('',#14006);
#4082=VERTEX_POINT('',#14008);
#4083=VERTEX_POINT('',#14012);
#4084=VERTEX_POINT('',#14013);
#4085=VERTEX_POINT('',#14018);
#4086=VERTEX_POINT('',#14020);
#4087=VERTEX_POINT('',#14024);
#4088=VERTEX_POINT('',#14025);
#4089=VERTEX_POINT('',#14027);
#4090=VERTEX_POINT('',#14029);
#4091=VERTEX_POINT('',#14036);
#4092=VERTEX_POINT('',#14041);
#4093=VERTEX_POINT('',#14063);
#4094=VERTEX_POINT('',#14067);
#4095=VERTEX_POINT('',#14094);
#4096=VERTEX_POINT('',#14096);
#4097=VERTEX_POINT('',#14100);
#4098=VERTEX_POINT('',#14102);
#4099=VERTEX_POINT('',#14110);
#4100=VERTEX_POINT('',#14112);
#4101=VERTEX_POINT('',#14116);
#4102=VERTEX_POINT('',#14118);
#4103=VERTEX_POINT('',#14122);
#4104=VERTEX_POINT('',#14124);
#4105=VERTEX_POINT('',#14128);
#4106=VERTEX_POINT('',#14130);
#4107=VERTEX_POINT('',#14139);
#4108=VERTEX_POINT('',#14141);
#4109=VERTEX_POINT('',#14145);
#4110=VERTEX_POINT('',#14147);
#4111=VERTEX_POINT('',#14155);
#4112=VERTEX_POINT('',#14157);
#4113=VERTEX_POINT('',#14161);
#4114=VERTEX_POINT('',#14163);
#4115=VERTEX_POINT('',#14167);
#4116=VERTEX_POINT('',#14169);
#4117=VERTEX_POINT('',#14173);
#4118=VERTEX_POINT('',#14175);
#4119=VERTEX_POINT('',#14185);
#4120=VERTEX_POINT('',#14187);
#4121=VERTEX_POINT('',#14191);
#4122=VERTEX_POINT('',#14193);
#4123=VERTEX_POINT('',#14197);
#4124=VERTEX_POINT('',#14199);
#4125=VERTEX_POINT('',#14203);
#4126=VERTEX_POINT('',#14205);
#4127=VERTEX_POINT('',#14209);
#4128=VERTEX_POINT('',#14211);
#4129=VERTEX_POINT('',#14215);
#4130=VERTEX_POINT('',#14217);
#4131=VERTEX_POINT('',#14221);
#4132=VERTEX_POINT('',#14223);
#4133=VERTEX_POINT('',#14227);
#4134=VERTEX_POINT('',#14229);
#4135=VERTEX_POINT('',#14233);
#4136=VERTEX_POINT('',#14234);
#4137=VERTEX_POINT('',#14236);
#4138=VERTEX_POINT('',#14238);
#4139=VERTEX_POINT('',#14242);
#4140=VERTEX_POINT('',#14243);
#4141=VERTEX_POINT('',#14245);
#4142=VERTEX_POINT('',#14247);
#4143=VERTEX_POINT('',#14251);
#4144=VERTEX_POINT('',#14254);
#4145=VERTEX_POINT('',#14258);
#4146=VERTEX_POINT('',#14259);
#4147=VERTEX_POINT('',#14261);
#4148=VERTEX_POINT('',#14263);
#4149=VERTEX_POINT('',#14267);
#4150=VERTEX_POINT('',#14268);
#4151=VERTEX_POINT('',#14271);
#4152=VERTEX_POINT('',#14275);
#4153=VERTEX_POINT('',#14277);
#4154=VERTEX_POINT('',#14279);
#4155=VERTEX_POINT('',#14283);
#4156=VERTEX_POINT('',#14284);
#4157=VERTEX_POINT('',#14286);
#4158=VERTEX_POINT('',#14288);
#4159=VERTEX_POINT('',#14292);
#4160=VERTEX_POINT('',#14294);
#4161=VERTEX_POINT('',#14298);
#4162=VERTEX_POINT('',#14299);
#4163=VERTEX_POINT('',#14301);
#4164=VERTEX_POINT('',#14303);
#4165=VERTEX_POINT('',#14307);
#4166=VERTEX_POINT('',#14309);
#4167=VERTEX_POINT('',#14316);
#4168=VERTEX_POINT('',#14317);
#4169=VERTEX_POINT('',#14325);
#4170=VERTEX_POINT('',#14326);
#4171=VERTEX_POINT('',#14331);
#4172=VERTEX_POINT('',#14333);
#4173=VERTEX_POINT('',#14337);
#4174=VERTEX_POINT('',#14339);
#4175=VERTEX_POINT('',#14343);
#4176=VERTEX_POINT('',#14344);
#4177=VERTEX_POINT('',#14349);
#4178=VERTEX_POINT('',#14351);
#4179=VERTEX_POINT('',#14355);
#4180=VERTEX_POINT('',#14356);
#4181=VERTEX_POINT('',#14358);
#4182=VERTEX_POINT('',#14360);
#4183=VERTEX_POINT('',#14367);
#4184=VERTEX_POINT('',#14368);
#4185=VERTEX_POINT('',#14373);
#4186=VERTEX_POINT('',#14375);
#4187=VERTEX_POINT('',#14379);
#4188=VERTEX_POINT('',#14380);
#4189=VERTEX_POINT('',#14382);
#4190=VERTEX_POINT('',#14384);
#4191=VERTEX_POINT('',#14391);
#4192=VERTEX_POINT('',#14396);
#4193=VERTEX_POINT('',#14418);
#4194=VERTEX_POINT('',#14422);
#4195=VERTEX_POINT('',#14449);
#4196=VERTEX_POINT('',#14451);
#4197=VERTEX_POINT('',#14455);
#4198=VERTEX_POINT('',#14457);
#4199=VERTEX_POINT('',#14465);
#4200=VERTEX_POINT('',#14467);
#4201=VERTEX_POINT('',#14471);
#4202=VERTEX_POINT('',#14473);
#4203=VERTEX_POINT('',#14477);
#4204=VERTEX_POINT('',#14479);
#4205=VERTEX_POINT('',#14483);
#4206=VERTEX_POINT('',#14485);
#4207=VERTEX_POINT('',#14494);
#4208=VERTEX_POINT('',#14496);
#4209=VERTEX_POINT('',#14500);
#4210=VERTEX_POINT('',#14502);
#4211=VERTEX_POINT('',#14510);
#4212=VERTEX_POINT('',#14512);
#4213=VERTEX_POINT('',#14516);
#4214=VERTEX_POINT('',#14518);
#4215=VERTEX_POINT('',#14522);
#4216=VERTEX_POINT('',#14524);
#4217=VERTEX_POINT('',#14528);
#4218=VERTEX_POINT('',#14530);
#4219=VERTEX_POINT('',#14540);
#4220=VERTEX_POINT('',#14542);
#4221=VERTEX_POINT('',#14546);
#4222=VERTEX_POINT('',#14548);
#4223=VERTEX_POINT('',#14552);
#4224=VERTEX_POINT('',#14554);
#4225=VERTEX_POINT('',#14558);
#4226=VERTEX_POINT('',#14560);
#4227=VERTEX_POINT('',#14564);
#4228=VERTEX_POINT('',#14566);
#4229=VERTEX_POINT('',#14570);
#4230=VERTEX_POINT('',#14572);
#4231=VERTEX_POINT('',#14576);
#4232=VERTEX_POINT('',#14578);
#4233=VERTEX_POINT('',#14582);
#4234=VERTEX_POINT('',#14584);
#4235=VERTEX_POINT('',#14588);
#4236=VERTEX_POINT('',#14589);
#4237=VERTEX_POINT('',#14591);
#4238=VERTEX_POINT('',#14593);
#4239=VERTEX_POINT('',#14597);
#4240=VERTEX_POINT('',#14598);
#4241=VERTEX_POINT('',#14600);
#4242=VERTEX_POINT('',#14602);
#4243=VERTEX_POINT('',#14606);
#4244=VERTEX_POINT('',#14608);
#4245=VERTEX_POINT('',#14612);
#4246=VERTEX_POINT('',#14613);
#4247=VERTEX_POINT('',#14615);
#4248=VERTEX_POINT('',#14617);
#4249=VERTEX_POINT('',#14621);
#4250=VERTEX_POINT('',#14623);
#4251=VERTEX_POINT('',#14627);
#4252=VERTEX_POINT('',#14628);
#4253=VERTEX_POINT('',#14630);
#4254=VERTEX_POINT('',#14632);
#4255=VERTEX_POINT('',#14642);
#4256=VERTEX_POINT('',#14643);
#4257=VERTEX_POINT('',#14648);
#4258=VERTEX_POINT('',#14649);
#4259=VERTEX_POINT('',#14651);
#4260=VERTEX_POINT('',#14653);
#4261=VERTEX_POINT('',#14657);
#4262=VERTEX_POINT('',#14659);
#4263=VERTEX_POINT('',#14663);
#4264=VERTEX_POINT('',#14665);
#4265=VERTEX_POINT('',#14669);
#4266=VERTEX_POINT('',#14671);
#4267=VERTEX_POINT('',#14675);
#4268=VERTEX_POINT('',#14679);
#4269=VERTEX_POINT('',#14689);
#4270=VERTEX_POINT('',#14693);
#4271=VERTEX_POINT('',#14706);
#4272=VERTEX_POINT('',#14708);
#4273=VERTEX_POINT('',#14710);
#4274=VERTEX_POINT('',#14712);
#4275=VERTEX_POINT('',#14727);
#4276=VERTEX_POINT('',#14729);
#4277=VERTEX_POINT('',#14733);
#4278=VERTEX_POINT('',#14735);
#4279=VERTEX_POINT('',#14739);
#4280=VERTEX_POINT('',#14741);
#4281=VERTEX_POINT('',#14745);
#4282=VERTEX_POINT('',#14747);
#4283=VERTEX_POINT('',#14751);
#4284=VERTEX_POINT('',#14753);
#4285=VERTEX_POINT('',#14757);
#4286=VERTEX_POINT('',#14759);
#4287=VERTEX_POINT('',#14763);
#4288=VERTEX_POINT('',#14765);
#4289=VERTEX_POINT('',#14769);
#4290=VERTEX_POINT('',#14771);
#4291=VERTEX_POINT('',#14775);
#4292=VERTEX_POINT('',#14776);
#4293=VERTEX_POINT('',#14778);
#4294=VERTEX_POINT('',#14780);
#4295=VERTEX_POINT('',#14784);
#4296=VERTEX_POINT('',#14785);
#4297=VERTEX_POINT('',#14787);
#4298=VERTEX_POINT('',#14789);
#4299=VERTEX_POINT('',#14793);
#4300=VERTEX_POINT('',#14795);
#4301=VERTEX_POINT('',#14799);
#4302=VERTEX_POINT('',#14800);
#4303=VERTEX_POINT('',#14802);
#4304=VERTEX_POINT('',#14804);
#4305=VERTEX_POINT('',#14808);
#4306=VERTEX_POINT('',#14810);
#4307=VERTEX_POINT('',#14814);
#4308=VERTEX_POINT('',#14815);
#4309=VERTEX_POINT('',#14817);
#4310=VERTEX_POINT('',#14819);
#4311=VERTEX_POINT('',#14829);
#4312=VERTEX_POINT('',#14830);
#4313=VERTEX_POINT('',#14835);
#4314=VERTEX_POINT('',#14836);
#4315=VERTEX_POINT('',#14838);
#4316=VERTEX_POINT('',#14840);
#4317=VERTEX_POINT('',#14844);
#4318=VERTEX_POINT('',#14846);
#4319=VERTEX_POINT('',#14850);
#4320=VERTEX_POINT('',#14852);
#4321=VERTEX_POINT('',#14856);
#4322=VERTEX_POINT('',#14858);
#4323=VERTEX_POINT('',#14862);
#4324=VERTEX_POINT('',#14864);
#4325=VERTEX_POINT('',#14876);
#4326=VERTEX_POINT('',#14880);
#4327=VERTEX_POINT('',#14893);
#4328=VERTEX_POINT('',#14895);
#4329=VERTEX_POINT('',#14897);
#4330=VERTEX_POINT('',#14899);
#4331=VERTEX_POINT('',#14914);
#4332=VERTEX_POINT('',#14916);
#4333=VERTEX_POINT('',#14920);
#4334=VERTEX_POINT('',#14922);
#4335=VERTEX_POINT('',#14926);
#4336=VERTEX_POINT('',#14928);
#4337=VERTEX_POINT('',#14932);
#4338=VERTEX_POINT('',#14933);
#4339=VERTEX_POINT('',#14935);
#4340=VERTEX_POINT('',#14937);
#4341=VERTEX_POINT('',#14941);
#4342=VERTEX_POINT('',#14943);
#4343=VERTEX_POINT('',#14947);
#4344=VERTEX_POINT('',#14948);
#4345=VERTEX_POINT('',#14950);
#4346=VERTEX_POINT('',#14952);
#4347=VERTEX_POINT('',#14956);
#4348=VERTEX_POINT('',#14958);
#4349=VERTEX_POINT('',#14962);
#4350=VERTEX_POINT('',#14963);
#4351=VERTEX_POINT('',#14968);
#4352=VERTEX_POINT('',#14970);
#4353=VERTEX_POINT('',#14974);
#4354=VERTEX_POINT('',#14975);
#4355=VERTEX_POINT('',#14977);
#4356=VERTEX_POINT('',#14979);
#4357=VERTEX_POINT('',#14986);
#4358=VERTEX_POINT('',#14987);
#4359=VERTEX_POINT('',#14992);
#4360=VERTEX_POINT('',#14993);
#4361=VERTEX_POINT('',#14998);
#4362=VERTEX_POINT('',#14999);
#4363=VERTEX_POINT('',#15001);
#4364=VERTEX_POINT('',#15003);
#4365=VERTEX_POINT('',#15010);
#4366=VERTEX_POINT('',#15011);
#4367=VERTEX_POINT('',#15016);
#4368=VERTEX_POINT('',#15017);
#4369=VERTEX_POINT('',#15019);
#4370=VERTEX_POINT('',#15021);
#4371=VERTEX_POINT('',#15025);
#4372=VERTEX_POINT('',#15027);
#4373=VERTEX_POINT('',#15031);
#4374=VERTEX_POINT('',#15033);
#4375=VERTEX_POINT('',#15037);
#4376=VERTEX_POINT('',#15039);
#4377=VERTEX_POINT('',#15043);
#4378=VERTEX_POINT('',#15045);
#4379=VERTEX_POINT('',#15061);
#4380=VERTEX_POINT('',#15065);
#4381=VERTEX_POINT('',#15082);
#4382=VERTEX_POINT('',#15083);
#4383=VERTEX_POINT('',#15085);
#4384=VERTEX_POINT('',#15088);
#4385=VERTEX_POINT('',#15103);
#4386=VERTEX_POINT('',#15104);
#4387=VERTEX_POINT('',#15106);
#4388=VERTEX_POINT('',#15108);
#4389=VERTEX_POINT('',#15112);
#4390=VERTEX_POINT('',#15114);
#4391=VERTEX_POINT('',#15118);
#4392=VERTEX_POINT('',#15119);
#4393=VERTEX_POINT('',#15121);
#4394=VERTEX_POINT('',#15123);
#4395=VERTEX_POINT('',#15127);
#4396=VERTEX_POINT('',#15129);
#4397=VERTEX_POINT('',#15133);
#4398=VERTEX_POINT('',#15134);
#4399=VERTEX_POINT('',#15139);
#4400=VERTEX_POINT('',#15141);
#4401=VERTEX_POINT('',#15145);
#4402=VERTEX_POINT('',#15146);
#4403=VERTEX_POINT('',#15148);
#4404=VERTEX_POINT('',#15150);
#4405=VERTEX_POINT('',#15157);
#4406=VERTEX_POINT('',#15162);
#4407=VERTEX_POINT('',#15175);
#4408=VERTEX_POINT('',#15179);
#4409=VERTEX_POINT('',#15196);
#4410=VERTEX_POINT('',#15197);
#4411=VERTEX_POINT('',#15199);
#4412=VERTEX_POINT('',#15214);
#4413=VERTEX_POINT('',#15231);
#4414=VERTEX_POINT('',#15232);
#4415=VERTEX_POINT('',#15236);
#4416=VERTEX_POINT('',#15237);
#4417=VERTEX_POINT('',#15251);
#4418=VERTEX_POINT('',#15253);
#4419=VERTEX_POINT('',#15255);
#4420=VERTEX_POINT('',#15257);
#4421=VERTEX_POINT('',#15271);
#4422=VERTEX_POINT('',#15273);
#4423=VERTEX_POINT('',#15284);
#4424=VERTEX_POINT('',#15286);
#4425=VERTEX_POINT('',#15288);
#4426=VERTEX_POINT('',#15290);
#4427=VERTEX_POINT('',#15292);
#4428=VERTEX_POINT('',#15294);
#4429=VERTEX_POINT('',#15306);
#4430=VERTEX_POINT('',#15307);
#4431=VERTEX_POINT('',#15321);
#4432=VERTEX_POINT('',#15323);
#4433=VERTEX_POINT('',#15334);
#4434=VERTEX_POINT('',#15336);
#4435=VERTEX_POINT('',#15349);
#4436=VERTEX_POINT('',#15351);
#4437=VERTEX_POINT('',#15363);
#4438=VERTEX_POINT('',#15364);
#4439=VERTEX_POINT('',#15366);
#4440=VERTEX_POINT('',#15368);
#4441=VERTEX_POINT('',#15371);
#4442=VERTEX_POINT('',#15372);
#4443=VERTEX_POINT('',#15386);
#4444=VERTEX_POINT('',#15388);
#4445=VERTEX_POINT('',#15399);
#4446=VERTEX_POINT('',#15401);
#4447=VERTEX_POINT('',#15414);
#4448=VERTEX_POINT('',#15416);
#4449=VERTEX_POINT('',#15427);
#4450=VERTEX_POINT('',#15429);
#4451=VERTEX_POINT('',#15431);
#4452=VERTEX_POINT('',#15433);
#4453=VERTEX_POINT('',#15444);
#4454=VERTEX_POINT('',#15446);
#4455=VERTEX_POINT('',#15459);
#4456=VERTEX_POINT('',#15461);
#4457=VERTEX_POINT('',#15472);
#4458=VERTEX_POINT('',#15474);
#4459=VERTEX_POINT('',#15488);
#4460=VERTEX_POINT('',#15490);
#4461=VERTEX_POINT('',#15493);
#4462=VERTEX_POINT('',#15494);
#4463=VERTEX_POINT('',#15508);
#4464=VERTEX_POINT('',#15510);
#4465=VERTEX_POINT('',#15521);
#4466=VERTEX_POINT('',#15523);
#4467=VERTEX_POINT('',#15536);
#4468=VERTEX_POINT('',#15538);
#4469=VERTEX_POINT('',#15550);
#4470=VERTEX_POINT('',#15551);
#4471=VERTEX_POINT('',#15564);
#4472=VERTEX_POINT('',#15566);
#4473=VERTEX_POINT('',#15577);
#4474=VERTEX_POINT('',#15579);
#4475=VERTEX_POINT('',#15593);
#4476=VERTEX_POINT('',#15595);
#4477=VERTEX_POINT('',#15597);
#4478=VERTEX_POINT('',#15599);
#4479=VERTEX_POINT('',#15649);
#4480=VERTEX_POINT('',#15651);
#4481=VERTEX_POINT('',#15683);
#4482=VERTEX_POINT('',#15685);
#4483=VERTEX_POINT('',#15698);
#4484=VERTEX_POINT('',#15700);
#4485=VERTEX_POINT('',#15714);
#4486=VERTEX_POINT('',#15716);
#4487=VERTEX_POINT('',#15727);
#4488=VERTEX_POINT('',#15729);
#4489=VERTEX_POINT('',#15742);
#4490=VERTEX_POINT('',#15744);
#4491=VERTEX_POINT('',#15746);
#4492=VERTEX_POINT('',#15748);
#4493=VERTEX_POINT('',#15761);
#4494=VERTEX_POINT('',#15763);
#4495=VERTEX_POINT('',#15795);
#4496=VERTEX_POINT('',#15797);
#4497=VERTEX_POINT('',#15846);
#4498=VERTEX_POINT('',#15848);
#4499=VERTEX_POINT('',#15863);
#4500=VERTEX_POINT('',#15864);
#4501=VERTEX_POINT('',#15877);
#4502=VERTEX_POINT('',#15879);
#4503=VERTEX_POINT('',#15894);
#4504=VERTEX_POINT('',#15896);
#4505=VERTEX_POINT('',#15911);
#4506=VERTEX_POINT('',#15913);
#4507=VERTEX_POINT('',#15928);
#4508=VERTEX_POINT('',#15929);
#4509=VERTEX_POINT('',#15942);
#4510=VERTEX_POINT('',#15944);
#4511=VERTEX_POINT('',#15959);
#4512=VERTEX_POINT('',#15961);
#4513=VERTEX_POINT('',#15976);
#4514=VERTEX_POINT('',#15978);
#4515=VERTEX_POINT('',#15993);
#4516=VERTEX_POINT('',#15995);
#4517=VERTEX_POINT('',#16010);
#4518=VERTEX_POINT('',#16012);
#4519=VERTEX_POINT('',#16027);
#4520=VERTEX_POINT('',#16029);
#4521=VERTEX_POINT('',#16044);
#4522=VERTEX_POINT('',#16046);
#4523=VERTEX_POINT('',#16050);
#4524=VERTEX_POINT('',#16051);
#4525=VERTEX_POINT('',#16053);
#4526=VERTEX_POINT('',#16068);
#4527=VERTEX_POINT('',#16085);
#4528=VERTEX_POINT('',#16087);
#4529=VERTEX_POINT('',#16091);
#4530=VERTEX_POINT('',#16093);
#4531=VERTEX_POINT('',#16097);
#4532=VERTEX_POINT('',#16099);
#4533=VERTEX_POINT('',#16103);
#4534=VERTEX_POINT('',#16105);
#4535=VERTEX_POINT('',#16108);
#4536=VERTEX_POINT('',#16110);
#4537=VERTEX_POINT('',#16114);
#4538=VERTEX_POINT('',#16115);
#4539=VERTEX_POINT('',#16117);
#4540=VERTEX_POINT('',#16119);
#4541=VERTEX_POINT('',#16121);
#4542=VERTEX_POINT('',#16123);
#4543=VERTEX_POINT('',#16125);
#4544=VERTEX_POINT('',#16127);
#4545=VERTEX_POINT('',#16129);
#4546=VERTEX_POINT('',#16131);
#4547=VERTEX_POINT('',#16133);
#4548=VERTEX_POINT('',#16135);
#4549=VERTEX_POINT('',#16161);
#4550=VERTEX_POINT('',#16163);
#4551=VERTEX_POINT('',#16199);
#4552=VERTEX_POINT('',#16201);
#4553=VERTEX_POINT('',#16252);
#4554=VERTEX_POINT('',#16254);
#4555=VERTEX_POINT('',#16267);
#4556=VERTEX_POINT('',#16269);
#4557=VERTEX_POINT('',#16285);
#4558=VERTEX_POINT('',#16287);
#4559=VERTEX_POINT('',#16339);
#4560=VERTEX_POINT('',#16343);
#4561=VERTEX_POINT('',#16349);
#4562=VERTEX_POINT('',#16351);
#4563=VERTEX_POINT('',#16389);
#4564=VERTEX_POINT('',#16391);
#4565=VERTEX_POINT('',#16407);
#4566=VERTEX_POINT('',#16409);
#4567=VERTEX_POINT('',#16422);
#4568=VERTEX_POINT('',#16426);
#4569=VERTEX_POINT('',#16445);
#4570=VERTEX_POINT('',#16447);
#4571=VERTEX_POINT('',#16460);
#4572=VERTEX_POINT('',#16462);
#4573=VERTEX_POINT('',#16478);
#4574=VERTEX_POINT('',#16480);
#4575=VERTEX_POINT('',#16501);
#4576=VERTEX_POINT('',#16503);
#4577=VERTEX_POINT('',#16505);
#4578=VERTEX_POINT('',#16537);
#4579=VERTEX_POINT('',#16539);
#4580=VERTEX_POINT('',#16589);
#4581=VERTEX_POINT('',#16623);
#4582=VERTEX_POINT('',#16627);
#4583=VERTEX_POINT('',#16631);
#4584=VERTEX_POINT('',#16665);
#4585=VERTEX_POINT('',#16669);
#4586=VERTEX_POINT('',#16721);
#4587=VERTEX_POINT('',#16761);
#4588=VERTEX_POINT('',#16763);
#4589=VERTEX_POINT('',#16776);
#4590=VERTEX_POINT('',#16778);
#4591=VERTEX_POINT('',#16794);
#4592=VERTEX_POINT('',#16796);
#4593=VERTEX_POINT('',#16812);
#4594=VERTEX_POINT('',#16816);
#4595=VERTEX_POINT('',#16822);
#4596=VERTEX_POINT('',#16824);
#4597=VERTEX_POINT('',#16841);
#4598=VERTEX_POINT('',#16843);
#4599=VERTEX_POINT('',#16858);
#4600=VERTEX_POINT('',#16860);
#4601=VERTEX_POINT('',#16877);
#4602=VERTEX_POINT('',#16881);
#4603=VERTEX_POINT('',#16890);
#4604=VERTEX_POINT('',#16892);
#4605=VERTEX_POINT('',#16905);
#4606=VERTEX_POINT('',#16907);
#4607=VERTEX_POINT('',#16923);
#4608=VERTEX_POINT('',#16925);
#4609=VERTEX_POINT('',#16941);
#4610=VERTEX_POINT('',#16945);
#4611=VERTEX_POINT('',#16951);
#4612=VERTEX_POINT('',#16953);
#4613=VERTEX_POINT('',#16968);
#4614=VERTEX_POINT('',#16970);
#4615=VERTEX_POINT('',#16974);
#4616=VERTEX_POINT('',#16980);
#4617=VERTEX_POINT('',#16989);
#4618=VERTEX_POINT('',#16991);
#4619=VERTEX_POINT('',#16995);
#4620=VERTEX_POINT('',#16999);
#4621=VERTEX_POINT('',#17006);
#4622=VERTEX_POINT('',#17008);
#4623=VERTEX_POINT('',#17012);
#4624=VERTEX_POINT('',#17044);
#4625=VERTEX_POINT('',#17081);
#4626=VERTEX_POINT('',#17083);
#4627=VERTEX_POINT('',#17087);
#4628=VERTEX_POINT('',#17101);
#4629=VERTEX_POINT('',#17117);
#4630=VERTEX_POINT('',#17119);
#4631=VERTEX_POINT('',#17123);
#4632=VERTEX_POINT('',#17155);
#4633=VERTEX_POINT('',#17196);
#4634=VERTEX_POINT('',#17198);
#4635=VERTEX_POINT('',#17200);
#4636=VERTEX_POINT('',#17211);
#4637=VERTEX_POINT('',#17213);
#4638=VERTEX_POINT('',#17227);
#4639=VERTEX_POINT('',#17256);
#4640=VERTEX_POINT('',#17258);
#4641=VERTEX_POINT('',#17262);
#4642=VERTEX_POINT('',#17266);
#4643=VERTEX_POINT('',#17270);
#4644=VERTEX_POINT('',#17271);
#4645=VERTEX_POINT('',#17274);
#4646=VERTEX_POINT('',#17278);
#4647=VERTEX_POINT('',#17282);
#4648=VERTEX_POINT('',#17283);
#4649=VERTEX_POINT('',#17287);
#4650=VERTEX_POINT('',#17293);
#4651=VERTEX_POINT('',#17294);
#4652=VERTEX_POINT('',#17296);
#4653=VERTEX_POINT('',#17299);
#4654=VERTEX_POINT('',#17303);
#4655=VERTEX_POINT('',#17311);
#4656=VERTEX_POINT('',#17319);
#4657=VERTEX_POINT('',#17327);
#4658=VERTEX_POINT('',#17335);
#4659=VERTEX_POINT('',#17343);
#4660=VERTEX_POINT('',#17345);
#4661=VERTEX_POINT('',#17349);
#4662=VERTEX_POINT('',#17353);
#4663=VERTEX_POINT('',#17357);
#4664=VERTEX_POINT('',#17361);
#4665=VERTEX_POINT('',#17371);
#4666=VERTEX_POINT('',#17373);
#4667=VERTEX_POINT('',#17377);
#4668=VERTEX_POINT('',#17379);
#4669=VERTEX_POINT('',#17381);
#4670=VERTEX_POINT('',#17385);
#4671=VERTEX_POINT('',#17386);
#4672=VERTEX_POINT('',#17391);
#4673=VERTEX_POINT('',#17393);
#4674=VERTEX_POINT('',#17397);
#4675=VERTEX_POINT('',#17401);
#4676=VERTEX_POINT('',#17403);
#4677=VERTEX_POINT('',#17407);
#4678=VERTEX_POINT('',#17409);
#4679=VERTEX_POINT('',#17413);
#4680=VERTEX_POINT('',#17417);
#4681=VERTEX_POINT('',#17419);
#4682=VERTEX_POINT('',#17421);
#4683=VERTEX_POINT('',#17425);
#4684=VERTEX_POINT('',#17426);
#4685=VERTEX_POINT('',#17431);
#4686=VERTEX_POINT('',#17443);
#4687=VERTEX_POINT('',#17445);
#4688=VERTEX_POINT('',#17447);
#4689=VERTEX_POINT('',#17449);
#4690=VERTEX_POINT('',#17451);
#4691=VERTEX_POINT('',#17453);
#4692=VERTEX_POINT('',#17455);
#4693=VERTEX_POINT('',#17459);
#4694=VERTEX_POINT('',#17460);
#4695=VERTEX_POINT('',#17462);
#4696=VERTEX_POINT('',#17467);
#4697=VERTEX_POINT('',#17471);
#4698=VERTEX_POINT('',#17475);
#4699=VERTEX_POINT('',#17476);
#4700=VERTEX_POINT('',#17480);
#4701=VERTEX_POINT('',#17486);
#4702=VERTEX_POINT('',#17487);
#4703=VERTEX_POINT('',#17489);
#4704=VERTEX_POINT('',#17492);
#4705=VERTEX_POINT('',#17496);
#4706=VERTEX_POINT('',#17504);
#4707=VERTEX_POINT('',#17512);
#4708=VERTEX_POINT('',#17520);
#4709=VERTEX_POINT('',#17528);
#4710=VERTEX_POINT('',#17536);
#4711=VERTEX_POINT('',#17539);
#4712=VERTEX_POINT('',#17543);
#4713=VERTEX_POINT('',#17548);
#4714=VERTEX_POINT('',#17553);
#4715=VERTEX_POINT('',#17558);
#4716=VERTEX_POINT('',#17574);
#4717=VERTEX_POINT('',#17575);
#4718=VERTEX_POINT('',#17577);
#4719=VERTEX_POINT('',#17579);
#4720=VERTEX_POINT('',#17581);
#4721=VERTEX_POINT('',#17585);
#4722=VERTEX_POINT('',#17588);
#4723=VERTEX_POINT('',#17590);
#4724=VERTEX_POINT('',#17594);
#4725=VERTEX_POINT('',#17596);
#4726=VERTEX_POINT('',#17600);
#4727=VERTEX_POINT('',#17604);
#4728=VERTEX_POINT('',#17606);
#4729=VERTEX_POINT('',#17610);
#4730=VERTEX_POINT('',#17614);
#4731=VERTEX_POINT('',#17618);
#4732=VERTEX_POINT('',#17622);
#4733=VERTEX_POINT('',#17623);
#4734=VERTEX_POINT('',#17626);
#4735=VERTEX_POINT('',#17630);
#4736=VERTEX_POINT('',#17634);
#4737=VERTEX_POINT('',#17636);
#4738=VERTEX_POINT('',#17640);
#4739=VERTEX_POINT('',#17644);
#4740=VERTEX_POINT('',#17659);
#4741=VERTEX_POINT('',#17661);
#4742=VERTEX_POINT('',#17665);
#4743=VERTEX_POINT('',#17666);
#4744=VERTEX_POINT('',#17671);
#4745=VERTEX_POINT('',#17673);
#4746=VERTEX_POINT('',#17677);
#4747=VERTEX_POINT('',#17679);
#4748=VERTEX_POINT('',#17681);
#4749=VERTEX_POINT('',#17687);
#4750=VERTEX_POINT('',#17691);
#4751=VERTEX_POINT('',#17695);
#4752=VERTEX_POINT('',#17697);
#4753=VERTEX_POINT('',#17701);
#4754=VERTEX_POINT('',#17703);
#4755=VERTEX_POINT('',#17707);
#4756=VERTEX_POINT('',#17708);
#4757=VERTEX_POINT('',#17713);
#4758=VERTEX_POINT('',#17717);
#4759=VERTEX_POINT('',#17718);
#4760=VERTEX_POINT('',#17720);
#4761=VERTEX_POINT('',#17722);
#4762=VERTEX_POINT('',#17726);
#4763=VERTEX_POINT('',#17728);
#4764=VERTEX_POINT('',#17732);
#4765=VERTEX_POINT('',#17734);
#4766=VERTEX_POINT('',#17738);
#4767=VERTEX_POINT('',#17740);
#4768=VERTEX_POINT('',#17744);
#4769=VERTEX_POINT('',#17746);
#4770=VERTEX_POINT('',#17750);
#4771=VERTEX_POINT('',#17752);
#4772=VERTEX_POINT('',#17756);
#4773=VERTEX_POINT('',#17758);
#4774=VERTEX_POINT('',#17770);
#4775=VERTEX_POINT('',#17772);
#4776=VERTEX_POINT('',#17776);
#4777=VERTEX_POINT('',#17778);
#4778=VERTEX_POINT('',#17782);
#4779=VERTEX_POINT('',#17784);
#4780=VERTEX_POINT('',#17788);
#4781=VERTEX_POINT('',#17790);
#4782=VERTEX_POINT('',#17794);
#4783=VERTEX_POINT('',#17798);
#4784=VERTEX_POINT('',#17802);
#4785=VERTEX_POINT('',#17804);
#4786=VERTEX_POINT('',#17808);
#4787=VERTEX_POINT('',#17810);
#4788=VERTEX_POINT('',#17814);
#4789=VERTEX_POINT('',#17816);
#4790=VERTEX_POINT('',#17820);
#4791=VERTEX_POINT('',#17822);
#4792=VERTEX_POINT('',#17835);
#4793=VERTEX_POINT('',#17837);
#4794=VERTEX_POINT('',#17841);
#4795=VERTEX_POINT('',#17843);
#4796=VERTEX_POINT('',#17847);
#4797=VERTEX_POINT('',#17851);
#4798=VERTEX_POINT('',#17855);
#4799=VERTEX_POINT('',#17857);
#4800=VERTEX_POINT('',#17861);
#4801=VERTEX_POINT('',#17863);
#4802=VERTEX_POINT('',#17865);
#4803=VERTEX_POINT('',#17869);
#4804=VERTEX_POINT('',#17870);
#4805=VERTEX_POINT('',#17875);
#4806=VERTEX_POINT('',#17877);
#4807=VERTEX_POINT('',#17881);
#4808=VERTEX_POINT('',#17882);
#4809=VERTEX_POINT('',#17887);
#4810=VERTEX_POINT('',#17891);
#4811=VERTEX_POINT('',#17895);
#4812=VERTEX_POINT('',#17899);
#4813=VERTEX_POINT('',#17908);
#4814=VERTEX_POINT('',#17910);
#4815=VERTEX_POINT('',#17914);
#4816=VERTEX_POINT('',#17916);
#4817=VERTEX_POINT('',#17923);
#4818=VERTEX_POINT('',#17924);
#4819=VERTEX_POINT('',#17926);
#4820=VERTEX_POINT('',#17931);
#4821=VERTEX_POINT('',#17935);
#4822=VERTEX_POINT('',#17939);
#4823=VERTEX_POINT('',#17941);
#4824=EDGE_CURVE('',#4013,#4013,#3564,.T.);
#4825=EDGE_CURVE('',#4013,#4014,#2116,.T.);
#4826=EDGE_CURVE('',#4014,#4014,#3565,.T.);
#4827=EDGE_CURVE('',#4015,#4015,#3566,.T.);
#4828=EDGE_CURVE('',#4015,#4016,#2117,.T.);
#4829=EDGE_CURVE('',#4016,#4016,#3567,.T.);
#4830=EDGE_CURVE('',#4017,#4017,#3568,.T.);
#4831=EDGE_CURVE('',#4017,#4018,#2118,.T.);
#4832=EDGE_CURVE('',#4018,#4018,#3569,.T.);
#4833=EDGE_CURVE('',#4019,#4019,#3570,.T.);
#4834=EDGE_CURVE('',#4019,#4020,#2119,.T.);
#4835=EDGE_CURVE('',#4020,#4020,#3571,.T.);
#4836=EDGE_CURVE('',#4021,#4021,#3572,.T.);
#4837=EDGE_CURVE('',#4021,#4022,#2120,.T.);
#4838=EDGE_CURVE('',#4022,#4022,#3573,.T.);
#4839=EDGE_CURVE('',#4023,#4023,#3574,.T.);
#4840=EDGE_CURVE('',#4023,#4024,#2121,.T.);
#4841=EDGE_CURVE('',#4024,#4024,#3575,.T.);
#4842=EDGE_CURVE('',#4025,#4025,#3576,.T.);
#4843=EDGE_CURVE('',#4025,#4026,#2122,.T.);
#4844=EDGE_CURVE('',#4026,#4026,#3577,.T.);
#4845=EDGE_CURVE('',#4027,#4027,#3578,.T.);
#4846=EDGE_CURVE('',#4027,#4028,#2123,.T.);
#4847=EDGE_CURVE('',#4028,#4028,#3579,.T.);
#4848=EDGE_CURVE('',#4029,#4029,#3580,.T.);
#4849=EDGE_CURVE('',#4029,#4030,#2124,.T.);
#4850=EDGE_CURVE('',#4030,#4030,#3581,.T.);
#4851=EDGE_CURVE('',#4031,#4031,#3582,.T.);
#4852=EDGE_CURVE('',#4031,#4032,#2125,.T.);
#4853=EDGE_CURVE('',#4032,#4032,#3583,.T.);
#4854=EDGE_CURVE('',#4033,#4033,#3584,.T.);
#4855=EDGE_CURVE('',#4033,#4034,#2126,.T.);
#4856=EDGE_CURVE('',#4034,#4034,#3585,.T.);
#4857=EDGE_CURVE('',#4035,#4036,#2127,.T.);
#4858=EDGE_CURVE('',#4036,#4037,#3586,.T.);
#4859=EDGE_CURVE('',#4038,#4037,#2128,.T.);
#4860=EDGE_CURVE('',#4038,#4035,#2129,.T.);
#4861=EDGE_CURVE('',#4039,#4040,#2130,.T.);
#4862=EDGE_CURVE('',#4039,#4041,#3587,.T.);
#4863=EDGE_CURVE('',#4041,#4042,#2131,.T.);
#4864=EDGE_CURVE('',#4042,#4040,#2132,.T.);
#4865=EDGE_CURVE('',#4043,#4037,#2133,.T.);
#4866=EDGE_CURVE('',#4037,#4039,#2134,.T.);
#4867=EDGE_CURVE('',#4044,#4039,#2135,.T.);
#4868=EDGE_CURVE('',#4044,#4043,#2136,.T.);
#4869=EDGE_CURVE('',#4045,#4046,#2137,.T.);
#4870=EDGE_CURVE('',#4047,#4045,#2138,.T.);
#4871=EDGE_CURVE('',#4048,#4047,#2139,.T.);
#4872=EDGE_CURVE('',#4048,#4046,#2140,.T.);
#4873=EDGE_CURVE('',#4049,#4050,#2141,.T.);
#4874=EDGE_CURVE('',#4050,#4044,#3588,.T.);
#4875=EDGE_CURVE('',#4051,#4044,#2142,.T.);
#4876=EDGE_CURVE('',#4051,#4049,#2143,.T.);
#4877=EDGE_CURVE('',#4052,#4043,#2144,.T.);
#4878=EDGE_CURVE('',#4043,#4053,#3589,.T.);
#4879=EDGE_CURVE('',#4054,#4053,#2145,.T.);
#4880=EDGE_CURVE('',#4054,#4052,#2146,.T.);
#4881=EDGE_CURVE('',#4055,#4056,#2147,.T.);
#4882=EDGE_CURVE('',#4057,#4055,#3590,.T.);
#4883=EDGE_CURVE('',#4058,#4057,#2148,.T.);
#4884=EDGE_CURVE('',#4058,#4056,#3591,.T.);
#4885=EDGE_CURVE('',#4055,#4059,#2149,.T.);
#4886=EDGE_CURVE('',#4056,#4060,#2150,.T.);
#4887=EDGE_CURVE('',#4060,#4059,#2151,.T.);
#4888=EDGE_CURVE('',#4061,#4062,#2152,.T.);
#4889=EDGE_CURVE('',#4061,#4063,#3592,.T.);
#4890=EDGE_CURVE('',#4064,#4063,#2153,.T.);
#4891=EDGE_CURVE('',#4062,#4064,#3593,.T.);
#4892=EDGE_CURVE('',#4065,#4061,#2154,.T.);
#4893=EDGE_CURVE('',#4066,#4062,#2155,.T.);
#4894=EDGE_CURVE('',#4066,#4065,#2156,.T.);
#4895=EDGE_CURVE('',#4067,#4068,#2157,.T.);
#4896=EDGE_CURVE('',#4059,#4067,#3594,.T.);
#4897=EDGE_CURVE('',#4060,#4068,#3595,.T.);
#4898=EDGE_CURVE('',#4067,#4069,#2158,.T.);
#4899=EDGE_CURVE('',#4068,#4070,#2159,.T.);
#4900=EDGE_CURVE('',#4070,#4069,#2160,.T.);
#4901=EDGE_CURVE('',#4071,#4072,#2161,.T.);
#4902=EDGE_CURVE('',#4071,#4073,#3596,.T.);
#4903=EDGE_CURVE('',#4074,#4073,#2162,.T.);
#4904=EDGE_CURVE('',#4072,#4074,#3597,.T.);
#4905=EDGE_CURVE('',#4063,#4071,#2163,.T.);
#4906=EDGE_CURVE('',#4064,#4072,#2164,.T.);
#4907=EDGE_CURVE('',#4069,#4051,#3598,.T.);
#4908=EDGE_CURVE('',#4070,#4049,#3599,.T.);
#4909=EDGE_CURVE('',#4075,#4076,#2165,.T.);
#4910=EDGE_CURVE('',#4075,#4040,#3600,.T.);
#4911=EDGE_CURVE('',#4076,#4042,#3601,.T.);
#4912=EDGE_CURVE('',#4073,#4075,#2166,.T.);
#4913=EDGE_CURVE('',#4074,#4076,#2167,.T.);
#4914=EDGE_CURVE('',#4077,#4078,#2168,.T.);
#4915=EDGE_CURVE('',#4052,#4077,#3602,.T.);
#4916=EDGE_CURVE('',#4054,#4078,#3603,.T.);
#4917=EDGE_CURVE('',#4077,#4079,#2169,.T.);
#4918=EDGE_CURVE('',#4078,#4080,#2170,.T.);
#4919=EDGE_CURVE('',#4080,#4079,#2171,.T.);
#4920=EDGE_CURVE('',#4038,#4081,#3604,.T.);
#4921=EDGE_CURVE('',#4082,#4081,#2172,.T.);
#4922=EDGE_CURVE('',#4035,#4082,#3605,.T.);
#4923=EDGE_CURVE('',#4083,#4084,#2173,.T.);
#4924=EDGE_CURVE('',#4079,#4083,#3606,.T.);
#4925=EDGE_CURVE('',#4080,#4084,#3607,.T.);
#4926=EDGE_CURVE('',#4083,#4085,#2174,.T.);
#4927=EDGE_CURVE('',#4084,#4086,#2175,.T.);
#4928=EDGE_CURVE('',#4085,#4086,#2176,.T.);
#4929=EDGE_CURVE('',#4087,#4088,#2177,.T.);
#4930=EDGE_CURVE('',#4087,#4089,#3608,.T.);
#4931=EDGE_CURVE('',#4090,#4089,#2178,.T.);
#4932=EDGE_CURVE('',#4088,#4090,#3609,.T.);
#4933=EDGE_CURVE('',#4081,#4087,#2179,.T.);
#4934=EDGE_CURVE('',#4082,#4088,#2180,.T.);
#4935=EDGE_CURVE('',#4090,#4091,#2181,.T.);
#4936=EDGE_CURVE('',#4086,#4091,#2182,.T.);
#4937=EDGE_CURVE('',#4084,#4090,#2183,.T.);
#4938=EDGE_CURVE('',#4092,#4091,#2184,.T.);
#4939=EDGE_CURVE('',#4085,#4092,#2185,.T.);
#4940=EDGE_CURVE('',#4089,#4092,#2186,.T.);
#4941=EDGE_CURVE('',#4083,#4089,#2187,.T.);
#4942=EDGE_CURVE('',#4079,#4087,#2188,.T.);
#4943=EDGE_CURVE('',#4077,#4081,#2189,.T.);
#4944=EDGE_CURVE('',#4069,#4075,#2190,.T.);
#4945=EDGE_CURVE('',#4067,#4073,#2191,.T.);
#4946=EDGE_CURVE('',#4059,#4071,#2192,.T.);
#4947=EDGE_CURVE('',#4055,#4063,#2193,.T.);
#4948=EDGE_CURVE('',#4057,#4061,#2194,.T.);
#4949=EDGE_CURVE('',#4093,#4065,#2195,.T.);
#4950=EDGE_CURVE('',#4093,#4057,#2196,.T.);
#4951=EDGE_CURVE('',#4094,#4066,#2197,.T.);
#4952=EDGE_CURVE('',#4094,#4093,#2198,.T.);
#4953=EDGE_CURVE('',#4058,#4062,#2199,.T.);
#4954=EDGE_CURVE('',#4094,#4058,#2200,.T.);
#4955=EDGE_CURVE('',#4056,#4064,#2201,.T.);
#4956=EDGE_CURVE('',#4060,#4072,#2202,.T.);
#4957=EDGE_CURVE('',#4068,#4074,#2203,.T.);
#4958=EDGE_CURVE('',#4070,#4076,#2204,.T.);
#4959=EDGE_CURVE('',#4046,#4041,#2205,.T.);
#4960=EDGE_CURVE('',#4050,#4048,#2206,.T.);
#4961=EDGE_CURVE('',#4078,#4082,#2207,.T.);
#4962=EDGE_CURVE('',#4053,#4047,#2208,.T.);
#4963=EDGE_CURVE('',#4036,#4045,#2209,.T.);
#4964=EDGE_CURVE('',#4080,#4088,#2210,.T.);
#4965=EDGE_CURVE('',#4053,#4095,#3610,.T.);
#4966=EDGE_CURVE('',#4096,#4095,#2211,.T.);
#4967=EDGE_CURVE('',#4047,#4096,#3611,.T.);
#4968=EDGE_CURVE('',#4097,#4050,#3612,.T.);
#4969=EDGE_CURVE('',#4098,#4048,#3613,.T.);
#4970=EDGE_CURVE('',#4098,#4097,#2212,.T.);
#4971=EDGE_CURVE('',#4097,#4095,#2213,.T.);
#4972=EDGE_CURVE('',#4096,#4098,#2214,.T.);
#4973=EDGE_CURVE('',#4098,#4099,#2215,.T.);
#4974=EDGE_CURVE('',#4099,#4100,#2216,.T.);
#4975=EDGE_CURVE('',#4097,#4100,#2217,.T.);
#4976=EDGE_CURVE('',#4101,#4095,#2218,.T.);
#4977=EDGE_CURVE('',#4101,#4102,#2219,.T.);
#4978=EDGE_CURVE('',#4102,#4096,#2220,.T.);
#4979=EDGE_CURVE('',#4100,#4103,#2221,.T.);
#4980=EDGE_CURVE('',#4103,#4104,#2222,.T.);
#4981=EDGE_CURVE('',#4104,#4101,#2223,.T.);
#4982=EDGE_CURVE('',#4105,#4102,#2224,.T.);
#4983=EDGE_CURVE('',#4106,#4105,#2225,.T.);
#4984=EDGE_CURVE('',#4099,#4106,#2226,.T.);
#4985=EDGE_CURVE('',#4105,#4104,#2227,.T.);
#4986=EDGE_CURVE('',#4106,#4103,#2228,.T.);
#4987=EDGE_CURVE('',#4046,#4107,#3614,.T.);
#4988=EDGE_CURVE('',#4041,#4108,#3615,.T.);
#4989=EDGE_CURVE('',#4107,#4108,#2229,.T.);
#4990=EDGE_CURVE('',#4109,#4036,#3616,.T.);
#4991=EDGE_CURVE('',#4110,#4045,#3617,.T.);
#4992=EDGE_CURVE('',#4110,#4109,#2230,.T.);
#4993=EDGE_CURVE('',#4109,#4108,#2231,.T.);
#4994=EDGE_CURVE('',#4107,#4110,#2232,.T.);
#4995=EDGE_CURVE('',#4111,#4108,#2233,.T.);
#4996=EDGE_CURVE('',#4112,#4111,#2234,.T.);
#4997=EDGE_CURVE('',#4112,#4107,#2235,.T.);
#4998=EDGE_CURVE('',#4110,#4113,#2236,.T.);
#4999=EDGE_CURVE('',#4114,#4113,#2237,.T.);
#5000=EDGE_CURVE('',#4109,#4114,#2238,.T.);
#5001=EDGE_CURVE('',#4114,#4115,#2239,.T.);
#5002=EDGE_CURVE('',#4115,#4116,#2240,.T.);
#5003=EDGE_CURVE('',#4116,#4111,#2241,.T.);
#5004=EDGE_CURVE('',#4117,#4112,#2242,.T.);
#5005=EDGE_CURVE('',#4118,#4117,#2243,.T.);
#5006=EDGE_CURVE('',#4113,#4118,#2244,.T.);
#5007=EDGE_CURVE('',#4118,#4115,#2245,.T.);
#5008=EDGE_CURVE('',#4117,#4116,#2246,.T.);
#5009=EDGE_CURVE('',#4119,#4119,#3618,.T.);
#5010=EDGE_CURVE('',#4119,#4120,#2247,.T.);
#5011=EDGE_CURVE('',#4120,#4120,#3619,.T.);
#5012=EDGE_CURVE('',#4121,#4121,#3620,.T.);
#5013=EDGE_CURVE('',#4121,#4122,#2248,.T.);
#5014=EDGE_CURVE('',#4122,#4122,#3621,.T.);
#5015=EDGE_CURVE('',#4123,#4123,#3622,.T.);
#5016=EDGE_CURVE('',#4123,#4124,#2249,.T.);
#5017=EDGE_CURVE('',#4124,#4124,#3623,.T.);
#5018=EDGE_CURVE('',#4125,#4125,#3624,.T.);
#5019=EDGE_CURVE('',#4125,#4126,#2250,.T.);
#5020=EDGE_CURVE('',#4126,#4126,#3625,.T.);
#5021=EDGE_CURVE('',#4127,#4127,#3626,.T.);
#5022=EDGE_CURVE('',#4127,#4128,#2251,.T.);
#5023=EDGE_CURVE('',#4128,#4128,#3627,.T.);
#5024=EDGE_CURVE('',#4129,#4129,#3628,.T.);
#5025=EDGE_CURVE('',#4129,#4130,#2252,.T.);
#5026=EDGE_CURVE('',#4130,#4130,#3629,.T.);
#5027=EDGE_CURVE('',#4131,#4131,#3630,.T.);
#5028=EDGE_CURVE('',#4131,#4132,#2253,.T.);
#5029=EDGE_CURVE('',#4132,#4132,#3631,.T.);
#5030=EDGE_CURVE('',#4133,#4133,#3632,.T.);
#5031=EDGE_CURVE('',#4133,#4134,#2254,.T.);
#5032=EDGE_CURVE('',#4134,#4134,#3633,.T.);
#5033=EDGE_CURVE('',#4135,#4136,#2255,.T.);
#5034=EDGE_CURVE('',#4136,#4137,#3634,.T.);
#5035=EDGE_CURVE('',#4138,#4137,#2256,.T.);
#5036=EDGE_CURVE('',#4138,#4135,#2257,.T.);
#5037=EDGE_CURVE('',#4139,#4140,#2258,.T.);
#5038=EDGE_CURVE('',#4139,#4141,#3635,.T.);
#5039=EDGE_CURVE('',#4141,#4142,#2259,.T.);
#5040=EDGE_CURVE('',#4142,#4140,#2260,.T.);
#5041=EDGE_CURVE('',#4143,#4137,#2261,.T.);
#5042=EDGE_CURVE('',#4137,#4139,#2262,.T.);
#5043=EDGE_CURVE('',#4144,#4139,#2263,.T.);
#5044=EDGE_CURVE('',#4144,#4143,#2264,.T.);
#5045=EDGE_CURVE('',#4145,#4146,#2265,.T.);
#5046=EDGE_CURVE('',#4147,#4145,#2266,.T.);
#5047=EDGE_CURVE('',#4148,#4147,#2267,.T.);
#5048=EDGE_CURVE('',#4148,#4146,#2268,.T.);
#5049=EDGE_CURVE('',#4149,#4150,#2269,.T.);
#5050=EDGE_CURVE('',#4150,#4144,#3636,.T.);
#5051=EDGE_CURVE('',#4151,#4144,#2270,.T.);
#5052=EDGE_CURVE('',#4151,#4149,#2271,.T.);
#5053=EDGE_CURVE('',#4152,#4143,#2272,.T.);
#5054=EDGE_CURVE('',#4143,#4153,#3637,.T.);
#5055=EDGE_CURVE('',#4154,#4153,#2273,.T.);
#5056=EDGE_CURVE('',#4154,#4152,#2274,.T.);
#5057=EDGE_CURVE('',#4155,#4156,#2275,.T.);
#5058=EDGE_CURVE('',#4157,#4155,#3638,.T.);
#5059=EDGE_CURVE('',#4158,#4157,#2276,.T.);
#5060=EDGE_CURVE('',#4158,#4156,#3639,.T.);
#5061=EDGE_CURVE('',#4155,#4159,#2277,.T.);
#5062=EDGE_CURVE('',#4156,#4160,#2278,.T.);
#5063=EDGE_CURVE('',#4160,#4159,#2279,.T.);
#5064=EDGE_CURVE('',#4161,#4162,#2280,.T.);
#5065=EDGE_CURVE('',#4161,#4163,#3640,.T.);
#5066=EDGE_CURVE('',#4164,#4163,#2281,.T.);
#5067=EDGE_CURVE('',#4162,#4164,#3641,.T.);
#5068=EDGE_CURVE('',#4165,#4161,#2282,.T.);
#5069=EDGE_CURVE('',#4166,#4162,#2283,.T.);
#5070=EDGE_CURVE('',#4166,#4165,#2284,.T.);
#5071=EDGE_CURVE('',#4159,#4151,#3642,.T.);
#5072=EDGE_CURVE('',#4160,#4149,#3643,.T.);
#5073=EDGE_CURVE('',#4167,#4168,#2285,.T.);
#5074=EDGE_CURVE('',#4167,#4140,#3644,.T.);
#5075=EDGE_CURVE('',#4168,#4142,#3645,.T.);
#5076=EDGE_CURVE('',#4163,#4167,#2286,.T.);
#5077=EDGE_CURVE('',#4164,#4168,#2287,.T.);
#5078=EDGE_CURVE('',#4169,#4170,#2288,.T.);
#5079=EDGE_CURVE('',#4152,#4169,#3646,.T.);
#5080=EDGE_CURVE('',#4154,#4170,#3647,.T.);
#5081=EDGE_CURVE('',#4169,#4171,#2289,.T.);
#5082=EDGE_CURVE('',#4170,#4172,#2290,.T.);
#5083=EDGE_CURVE('',#4172,#4171,#2291,.T.);
#5084=EDGE_CURVE('',#4138,#4173,#3648,.T.);
#5085=EDGE_CURVE('',#4174,#4173,#2292,.T.);
#5086=EDGE_CURVE('',#4135,#4174,#3649,.T.);
#5087=EDGE_CURVE('',#4175,#4176,#2293,.T.);
#5088=EDGE_CURVE('',#4171,#4175,#3650,.T.);
#5089=EDGE_CURVE('',#4172,#4176,#3651,.T.);
#5090=EDGE_CURVE('',#4175,#4177,#2294,.T.);
#5091=EDGE_CURVE('',#4176,#4178,#2295,.T.);
#5092=EDGE_CURVE('',#4178,#4177,#2296,.T.);
#5093=EDGE_CURVE('',#4179,#4180,#2297,.T.);
#5094=EDGE_CURVE('',#4179,#4181,#3652,.T.);
#5095=EDGE_CURVE('',#4182,#4181,#2298,.T.);
#5096=EDGE_CURVE('',#4180,#4182,#3653,.T.);
#5097=EDGE_CURVE('',#4173,#4179,#2299,.T.);
#5098=EDGE_CURVE('',#4174,#4180,#2300,.T.);
#5099=EDGE_CURVE('',#4183,#4184,#2301,.T.);
#5100=EDGE_CURVE('',#4177,#4183,#3654,.T.);
#5101=EDGE_CURVE('',#4178,#4184,#3655,.T.);
#5102=EDGE_CURVE('',#4183,#4185,#2302,.T.);
#5103=EDGE_CURVE('',#4184,#4186,#2303,.T.);
#5104=EDGE_CURVE('',#4185,#4186,#2304,.T.);
#5105=EDGE_CURVE('',#4187,#4188,#2305,.T.);
#5106=EDGE_CURVE('',#4187,#4189,#3656,.T.);
#5107=EDGE_CURVE('',#4190,#4189,#2306,.T.);
#5108=EDGE_CURVE('',#4188,#4190,#3657,.T.);
#5109=EDGE_CURVE('',#4181,#4187,#2307,.T.);
#5110=EDGE_CURVE('',#4182,#4188,#2308,.T.);
#5111=EDGE_CURVE('',#4190,#4191,#2309,.T.);
#5112=EDGE_CURVE('',#4186,#4191,#2310,.T.);
#5113=EDGE_CURVE('',#4184,#4190,#2311,.T.);
#5114=EDGE_CURVE('',#4192,#4191,#2312,.T.);
#5115=EDGE_CURVE('',#4185,#4192,#2313,.T.);
#5116=EDGE_CURVE('',#4189,#4192,#2314,.T.);
#5117=EDGE_CURVE('',#4183,#4189,#2315,.T.);
#5118=EDGE_CURVE('',#4177,#4187,#2316,.T.);
#5119=EDGE_CURVE('',#4175,#4181,#2317,.T.);
#5120=EDGE_CURVE('',#4171,#4179,#2318,.T.);
#5121=EDGE_CURVE('',#4169,#4173,#2319,.T.);
#5122=EDGE_CURVE('',#4159,#4167,#2320,.T.);
#5123=EDGE_CURVE('',#4155,#4163,#2321,.T.);
#5124=EDGE_CURVE('',#4157,#4161,#2322,.T.);
#5125=EDGE_CURVE('',#4193,#4165,#2323,.T.);
#5126=EDGE_CURVE('',#4193,#4157,#2324,.T.);
#5127=EDGE_CURVE('',#4194,#4166,#2325,.T.);
#5128=EDGE_CURVE('',#4194,#4193,#2326,.T.);
#5129=EDGE_CURVE('',#4158,#4162,#2327,.T.);
#5130=EDGE_CURVE('',#4194,#4158,#2328,.T.);
#5131=EDGE_CURVE('',#4156,#4164,#2329,.T.);
#5132=EDGE_CURVE('',#4160,#4168,#2330,.T.);
#5133=EDGE_CURVE('',#4146,#4141,#2331,.T.);
#5134=EDGE_CURVE('',#4150,#4148,#2332,.T.);
#5135=EDGE_CURVE('',#4170,#4174,#2333,.T.);
#5136=EDGE_CURVE('',#4153,#4147,#2334,.T.);
#5137=EDGE_CURVE('',#4136,#4145,#2335,.T.);
#5138=EDGE_CURVE('',#4172,#4180,#2336,.T.);
#5139=EDGE_CURVE('',#4176,#4182,#2337,.T.);
#5140=EDGE_CURVE('',#4178,#4188,#2338,.T.);
#5141=EDGE_CURVE('',#4153,#4195,#3658,.T.);
#5142=EDGE_CURVE('',#4196,#4195,#2339,.T.);
#5143=EDGE_CURVE('',#4147,#4196,#3659,.T.);
#5144=EDGE_CURVE('',#4197,#4150,#3660,.T.);
#5145=EDGE_CURVE('',#4198,#4148,#3661,.T.);
#5146=EDGE_CURVE('',#4198,#4197,#2340,.T.);
#5147=EDGE_CURVE('',#4197,#4195,#2341,.T.);
#5148=EDGE_CURVE('',#4196,#4198,#2342,.T.);
#5149=EDGE_CURVE('',#4198,#4199,#2343,.T.);
#5150=EDGE_CURVE('',#4200,#4199,#2344,.T.);
#5151=EDGE_CURVE('',#4197,#4200,#2345,.T.);
#5152=EDGE_CURVE('',#4201,#4195,#2346,.T.);
#5153=EDGE_CURVE('',#4202,#4201,#2347,.T.);
#5154=EDGE_CURVE('',#4202,#4196,#2348,.T.);
#5155=EDGE_CURVE('',#4200,#4203,#2349,.T.);
#5156=EDGE_CURVE('',#4203,#4204,#2350,.T.);
#5157=EDGE_CURVE('',#4204,#4201,#2351,.T.);
#5158=EDGE_CURVE('',#4205,#4202,#2352,.T.);
#5159=EDGE_CURVE('',#4206,#4205,#2353,.T.);
#5160=EDGE_CURVE('',#4199,#4206,#2354,.T.);
#5161=EDGE_CURVE('',#4206,#4203,#2355,.T.);
#5162=EDGE_CURVE('',#4205,#4204,#2356,.T.);
#5163=EDGE_CURVE('',#4146,#4207,#3662,.T.);
#5164=EDGE_CURVE('',#4141,#4208,#3663,.T.);
#5165=EDGE_CURVE('',#4207,#4208,#2357,.T.);
#5166=EDGE_CURVE('',#4209,#4136,#3664,.T.);
#5167=EDGE_CURVE('',#4210,#4145,#3665,.T.);
#5168=EDGE_CURVE('',#4210,#4209,#2358,.T.);
#5169=EDGE_CURVE('',#4209,#4208,#2359,.T.);
#5170=EDGE_CURVE('',#4207,#4210,#2360,.T.);
#5171=EDGE_CURVE('',#4211,#4208,#2361,.T.);
#5172=EDGE_CURVE('',#4211,#4212,#2362,.T.);
#5173=EDGE_CURVE('',#4212,#4207,#2363,.T.);
#5174=EDGE_CURVE('',#4210,#4213,#2364,.T.);
#5175=EDGE_CURVE('',#4213,#4214,#2365,.T.);
#5176=EDGE_CURVE('',#4209,#4214,#2366,.T.);
#5177=EDGE_CURVE('',#4214,#4215,#2367,.T.);
#5178=EDGE_CURVE('',#4215,#4216,#2368,.T.);
#5179=EDGE_CURVE('',#4216,#4211,#2369,.T.);
#5180=EDGE_CURVE('',#4217,#4212,#2370,.T.);
#5181=EDGE_CURVE('',#4218,#4217,#2371,.T.);
#5182=EDGE_CURVE('',#4213,#4218,#2372,.T.);
#5183=EDGE_CURVE('',#4217,#4216,#2373,.T.);
#5184=EDGE_CURVE('',#4218,#4215,#2374,.T.);
#5185=EDGE_CURVE('',#4219,#4219,#3666,.T.);
#5186=EDGE_CURVE('',#4219,#4220,#2375,.T.);
#5187=EDGE_CURVE('',#4220,#4220,#3667,.T.);
#5188=EDGE_CURVE('',#4221,#4221,#3668,.T.);
#5189=EDGE_CURVE('',#4221,#4222,#2376,.T.);
#5190=EDGE_CURVE('',#4222,#4222,#3669,.T.);
#5191=EDGE_CURVE('',#4223,#4223,#3670,.T.);
#5192=EDGE_CURVE('',#4223,#4224,#2377,.T.);
#5193=EDGE_CURVE('',#4224,#4224,#3671,.T.);
#5194=EDGE_CURVE('',#4225,#4225,#3672,.T.);
#5195=EDGE_CURVE('',#4225,#4226,#2378,.T.);
#5196=EDGE_CURVE('',#4226,#4226,#3673,.T.);
#5197=EDGE_CURVE('',#4227,#4227,#3674,.T.);
#5198=EDGE_CURVE('',#4227,#4228,#2379,.T.);
#5199=EDGE_CURVE('',#4228,#4228,#3675,.T.);
#5200=EDGE_CURVE('',#4229,#4229,#3676,.T.);
#5201=EDGE_CURVE('',#4229,#4230,#2380,.T.);
#5202=EDGE_CURVE('',#4230,#4230,#3677,.T.);
#5203=EDGE_CURVE('',#4231,#4231,#3678,.T.);
#5204=EDGE_CURVE('',#4231,#4232,#2381,.T.);
#5205=EDGE_CURVE('',#4232,#4232,#3679,.T.);
#5206=EDGE_CURVE('',#4233,#4233,#3680,.T.);
#5207=EDGE_CURVE('',#4233,#4234,#2382,.T.);
#5208=EDGE_CURVE('',#4234,#4234,#3681,.T.);
#5209=EDGE_CURVE('',#4235,#4236,#2383,.T.);
#5210=EDGE_CURVE('',#4236,#4237,#2384,.T.);
#5211=EDGE_CURVE('',#4238,#4237,#2385,.T.);
#5212=EDGE_CURVE('',#4238,#4235,#2386,.T.);
#5213=EDGE_CURVE('',#4239,#4240,#2387,.T.);
#5214=EDGE_CURVE('',#4239,#4241,#3682,.T.);
#5215=EDGE_CURVE('',#4242,#4241,#2388,.T.);
#5216=EDGE_CURVE('',#4240,#4242,#3683,.T.);
#5217=EDGE_CURVE('',#4243,#4239,#2389,.T.);
#5218=EDGE_CURVE('',#4244,#4240,#2390,.T.);
#5219=EDGE_CURVE('',#4243,#4244,#2391,.T.);
#5220=EDGE_CURVE('',#4245,#4246,#2392,.T.);
#5221=EDGE_CURVE('',#4247,#4245,#3684,.T.);
#5222=EDGE_CURVE('',#4248,#4247,#2393,.T.);
#5223=EDGE_CURVE('',#4248,#4246,#3685,.T.);
#5224=EDGE_CURVE('',#4245,#4249,#2394,.T.);
#5225=EDGE_CURVE('',#4246,#4250,#2395,.T.);
#5226=EDGE_CURVE('',#4250,#4249,#2396,.T.);
#5227=EDGE_CURVE('',#4251,#4252,#2397,.T.);
#5228=EDGE_CURVE('',#4251,#4253,#3686,.T.);
#5229=EDGE_CURVE('',#4254,#4253,#2398,.T.);
#5230=EDGE_CURVE('',#4252,#4254,#3687,.T.);
#5231=EDGE_CURVE('',#4241,#4251,#2399,.T.);
#5232=EDGE_CURVE('',#4242,#4252,#2400,.T.);
#5233=EDGE_CURVE('',#4249,#4238,#3688,.T.);
#5234=EDGE_CURVE('',#4250,#4235,#3689,.T.);
#5235=EDGE_CURVE('',#4255,#4256,#2401,.T.);
#5236=EDGE_CURVE('',#4254,#4255,#2402,.T.);
#5237=EDGE_CURVE('',#4253,#4256,#2403,.T.);
#5238=EDGE_CURVE('',#4257,#4258,#2404,.T.);
#5239=EDGE_CURVE('',#4258,#4259,#2405,.T.);
#5240=EDGE_CURVE('',#4260,#4259,#2406,.T.);
#5241=EDGE_CURVE('',#4260,#4257,#2407,.T.);
#5242=EDGE_CURVE('',#4259,#4261,#2408,.T.);
#5243=EDGE_CURVE('',#4262,#4261,#2409,.T.);
#5244=EDGE_CURVE('',#4260,#4262,#2410,.T.);
#5245=EDGE_CURVE('',#4263,#4261,#2411,.T.);
#5246=EDGE_CURVE('',#4264,#4263,#2412,.T.);
#5247=EDGE_CURVE('',#4262,#4264,#2413,.T.);
#5248=EDGE_CURVE('',#4265,#4263,#268,.T.);
#5249=EDGE_CURVE('',#4266,#4265,#2414,.T.);
#5250=EDGE_CURVE('',#4264,#4266,#269,.T.);
#5251=EDGE_CURVE('',#4267,#4265,#2415,.T.);
#5252=EDGE_CURVE('',#4267,#4236,#2416,.T.);
#5253=EDGE_CURVE('',#4254,#4235,#2417,.T.);
#5254=EDGE_CURVE('',#4268,#4255,#2418,.T.);
#5255=EDGE_CURVE('',#4266,#4268,#2419,.T.);
#5256=EDGE_CURVE('',#4252,#4250,#2420,.T.);
#5257=EDGE_CURVE('',#4242,#4246,#2421,.T.);
#5258=EDGE_CURVE('',#4240,#4248,#2422,.T.);
#5259=EDGE_CURVE('',#4269,#4248,#2423,.T.);
#5260=EDGE_CURVE('',#4244,#4269,#2424,.T.);
#5261=EDGE_CURVE('',#4270,#4269,#2425,.T.);
#5262=EDGE_CURVE('',#4243,#4270,#2426,.T.);
#5263=EDGE_CURVE('',#4270,#4247,#2427,.T.);
#5264=EDGE_CURVE('',#4239,#4247,#2428,.T.);
#5265=EDGE_CURVE('',#4241,#4245,#2429,.T.);
#5266=EDGE_CURVE('',#4251,#4249,#2430,.T.);
#5267=EDGE_CURVE('',#4253,#4238,#2431,.T.);
#5268=EDGE_CURVE('',#4271,#4237,#2432,.T.);
#5269=EDGE_CURVE('',#4271,#4272,#2433,.T.);
#5270=EDGE_CURVE('',#4273,#4272,#2434,.T.);
#5271=EDGE_CURVE('',#4273,#4274,#2435,.T.);
#5272=EDGE_CURVE('',#4274,#4256,#2436,.T.);
#5273=EDGE_CURVE('',#4272,#4258,#270,.T.);
#5274=EDGE_CURVE('',#4257,#4273,#271,.T.);
#5275=EDGE_CURVE('',#4274,#4268,#2437,.T.);
#5276=EDGE_CURVE('',#4267,#4271,#2438,.T.);
#5277=EDGE_CURVE('',#4275,#4275,#3690,.T.);
#5278=EDGE_CURVE('',#4275,#4276,#2439,.T.);
#5279=EDGE_CURVE('',#4276,#4276,#3691,.T.);
#5280=EDGE_CURVE('',#4277,#4277,#3692,.T.);
#5281=EDGE_CURVE('',#4277,#4278,#2440,.T.);
#5282=EDGE_CURVE('',#4278,#4278,#3693,.T.);
#5283=EDGE_CURVE('',#4279,#4279,#3694,.T.);
#5284=EDGE_CURVE('',#4279,#4280,#2441,.T.);
#5285=EDGE_CURVE('',#4280,#4280,#3695,.T.);
#5286=EDGE_CURVE('',#4281,#4281,#3696,.T.);
#5287=EDGE_CURVE('',#4281,#4282,#2442,.T.);
#5288=EDGE_CURVE('',#4282,#4282,#3697,.T.);
#5289=EDGE_CURVE('',#4283,#4283,#3698,.T.);
#5290=EDGE_CURVE('',#4283,#4284,#2443,.T.);
#5291=EDGE_CURVE('',#4284,#4284,#3699,.T.);
#5292=EDGE_CURVE('',#4285,#4285,#3700,.T.);
#5293=EDGE_CURVE('',#4285,#4286,#2444,.T.);
#5294=EDGE_CURVE('',#4286,#4286,#3701,.T.);
#5295=EDGE_CURVE('',#4287,#4287,#3702,.T.);
#5296=EDGE_CURVE('',#4287,#4288,#2445,.T.);
#5297=EDGE_CURVE('',#4288,#4288,#3703,.T.);
#5298=EDGE_CURVE('',#4289,#4289,#3704,.T.);
#5299=EDGE_CURVE('',#4289,#4290,#2446,.T.);
#5300=EDGE_CURVE('',#4290,#4290,#3705,.T.);
#5301=EDGE_CURVE('',#4291,#4292,#2447,.T.);
#5302=EDGE_CURVE('',#4293,#4291,#2448,.T.);
#5303=EDGE_CURVE('',#4293,#4294,#2449,.T.);
#5304=EDGE_CURVE('',#4292,#4294,#2450,.T.);
#5305=EDGE_CURVE('',#4295,#4296,#2451,.T.);
#5306=EDGE_CURVE('',#4296,#4297,#3706,.T.);
#5307=EDGE_CURVE('',#4297,#4298,#2452,.T.);
#5308=EDGE_CURVE('',#4295,#4298,#3707,.T.);
#5309=EDGE_CURVE('',#4299,#4295,#2453,.T.);
#5310=EDGE_CURVE('',#4299,#4300,#2454,.T.);
#5311=EDGE_CURVE('',#4300,#4296,#2455,.T.);
#5312=EDGE_CURVE('',#4301,#4302,#2456,.T.);
#5313=EDGE_CURVE('',#4303,#4302,#3708,.T.);
#5314=EDGE_CURVE('',#4303,#4304,#2457,.T.);
#5315=EDGE_CURVE('',#4304,#4301,#3709,.T.);
#5316=EDGE_CURVE('',#4301,#4305,#2458,.T.);
#5317=EDGE_CURVE('',#4306,#4305,#2459,.T.);
#5318=EDGE_CURVE('',#4302,#4306,#2460,.T.);
#5319=EDGE_CURVE('',#4307,#4308,#2461,.T.);
#5320=EDGE_CURVE('',#4308,#4309,#3710,.T.);
#5321=EDGE_CURVE('',#4309,#4310,#2462,.T.);
#5322=EDGE_CURVE('',#4307,#4310,#3711,.T.);
#5323=EDGE_CURVE('',#4298,#4307,#2463,.T.);
#5324=EDGE_CURVE('',#4297,#4308,#2464,.T.);
#5325=EDGE_CURVE('',#4306,#4291,#3712,.T.);
#5326=EDGE_CURVE('',#4305,#4293,#3713,.T.);
#5327=EDGE_CURVE('',#4311,#4312,#2465,.T.);
#5328=EDGE_CURVE('',#4310,#4312,#2466,.T.);
#5329=EDGE_CURVE('',#4309,#4311,#2467,.T.);
#5330=EDGE_CURVE('',#4313,#4314,#2468,.T.);
#5331=EDGE_CURVE('',#4315,#4313,#2469,.T.);
#5332=EDGE_CURVE('',#4315,#4316,#2470,.T.);
#5333=EDGE_CURVE('',#4314,#4316,#2471,.T.);
#5334=EDGE_CURVE('',#4316,#4317,#2472,.T.);
#5335=EDGE_CURVE('',#4315,#4318,#2473,.T.);
#5336=EDGE_CURVE('',#4318,#4317,#2474,.T.);
#5337=EDGE_CURVE('',#4319,#4317,#2475,.T.);
#5338=EDGE_CURVE('',#4318,#4320,#2476,.T.);
#5339=EDGE_CURVE('',#4320,#4319,#2477,.T.);
#5340=EDGE_CURVE('',#4321,#4319,#272,.T.);
#5341=EDGE_CURVE('',#4320,#4322,#273,.T.);
#5342=EDGE_CURVE('',#4322,#4321,#2478,.T.);
#5343=EDGE_CURVE('',#4323,#4321,#2479,.T.);
#5344=EDGE_CURVE('',#4322,#4324,#2480,.T.);
#5345=EDGE_CURVE('',#4324,#4311,#2481,.T.);
#5346=EDGE_CURVE('',#4309,#4291,#2482,.T.);
#5347=EDGE_CURVE('',#4323,#4292,#2483,.T.);
#5348=EDGE_CURVE('',#4308,#4306,#2484,.T.);
#5349=EDGE_CURVE('',#4297,#4302,#2485,.T.);
#5350=EDGE_CURVE('',#4296,#4303,#2486,.T.);
#5351=EDGE_CURVE('',#4325,#4303,#2487,.T.);
#5352=EDGE_CURVE('',#4300,#4325,#2488,.T.);
#5353=EDGE_CURVE('',#4326,#4325,#2489,.T.);
#5354=EDGE_CURVE('',#4299,#4326,#2490,.T.);
#5355=EDGE_CURVE('',#4326,#4304,#2491,.T.);
#5356=EDGE_CURVE('',#4295,#4304,#2492,.T.);
#5357=EDGE_CURVE('',#4298,#4301,#2493,.T.);
#5358=EDGE_CURVE('',#4307,#4305,#2494,.T.);
#5359=EDGE_CURVE('',#4310,#4293,#2495,.T.);
#5360=EDGE_CURVE('',#4327,#4294,#2496,.T.);
#5361=EDGE_CURVE('',#4328,#4312,#2497,.T.);
#5362=EDGE_CURVE('',#4329,#4328,#2498,.T.);
#5363=EDGE_CURVE('',#4329,#4330,#2499,.T.);
#5364=EDGE_CURVE('',#4327,#4330,#2500,.T.);
#5365=EDGE_CURVE('',#4313,#4329,#274,.T.);
#5366=EDGE_CURVE('',#4330,#4314,#275,.T.);
#5367=EDGE_CURVE('',#4328,#4324,#2501,.T.);
#5368=EDGE_CURVE('',#4323,#4327,#2502,.T.);
#5369=EDGE_CURVE('',#4331,#4331,#3714,.T.);
#5370=EDGE_CURVE('',#4331,#4332,#2503,.T.);
#5371=EDGE_CURVE('',#4332,#4332,#3715,.T.);
#5372=EDGE_CURVE('',#4333,#4333,#3716,.T.);
#5373=EDGE_CURVE('',#4333,#4334,#2504,.T.);
#5374=EDGE_CURVE('',#4334,#4334,#3717,.T.);
#5375=EDGE_CURVE('',#4335,#4335,#3718,.T.);
#5376=EDGE_CURVE('',#4335,#4336,#2505,.T.);
#5377=EDGE_CURVE('',#4336,#4336,#3719,.T.);
#5378=EDGE_CURVE('',#4337,#4338,#2506,.T.);
#5379=EDGE_CURVE('',#4339,#4337,#3720,.T.);
#5380=EDGE_CURVE('',#4340,#4339,#2507,.T.);
#5381=EDGE_CURVE('',#4340,#4338,#3721,.T.);
#5382=EDGE_CURVE('',#4337,#4341,#2508,.T.);
#5383=EDGE_CURVE('',#4338,#4342,#2509,.T.);
#5384=EDGE_CURVE('',#4342,#4341,#2510,.T.);
#5385=EDGE_CURVE('',#4343,#4344,#2511,.T.);
#5386=EDGE_CURVE('',#4343,#4345,#3722,.T.);
#5387=EDGE_CURVE('',#4346,#4345,#2512,.T.);
#5388=EDGE_CURVE('',#4344,#4346,#3723,.T.);
#5389=EDGE_CURVE('',#4347,#4343,#2513,.T.);
#5390=EDGE_CURVE('',#4348,#4344,#2514,.T.);
#5391=EDGE_CURVE('',#4348,#4347,#2515,.T.);
#5392=EDGE_CURVE('',#4349,#4350,#2516,.T.);
#5393=EDGE_CURVE('',#4341,#4349,#3724,.T.);
#5394=EDGE_CURVE('',#4342,#4350,#3725,.T.);
#5395=EDGE_CURVE('',#4349,#4351,#2517,.T.);
#5396=EDGE_CURVE('',#4350,#4352,#2518,.T.);
#5397=EDGE_CURVE('',#4352,#4351,#2519,.T.);
#5398=EDGE_CURVE('',#4353,#4354,#2520,.T.);
#5399=EDGE_CURVE('',#4353,#4355,#3726,.T.);
#5400=EDGE_CURVE('',#4356,#4355,#2521,.T.);
#5401=EDGE_CURVE('',#4354,#4356,#3727,.T.);
#5402=EDGE_CURVE('',#4345,#4353,#2522,.T.);
#5403=EDGE_CURVE('',#4346,#4354,#2523,.T.);
#5404=EDGE_CURVE('',#4357,#4358,#2524,.T.);
#5405=EDGE_CURVE('',#4351,#4357,#3728,.T.);
#5406=EDGE_CURVE('',#4352,#4358,#3729,.T.);
#5407=EDGE_CURVE('',#4359,#4360,#2525,.T.);
#5408=EDGE_CURVE('',#4357,#4359,#2526,.T.);
#5409=EDGE_CURVE('',#4358,#4360,#2527,.T.);
#5410=EDGE_CURVE('',#4361,#4362,#2528,.T.);
#5411=EDGE_CURVE('',#4361,#4363,#3730,.T.);
#5412=EDGE_CURVE('',#4364,#4363,#2529,.T.);
#5413=EDGE_CURVE('',#4362,#4364,#3731,.T.);
#5414=EDGE_CURVE('',#4355,#4361,#2530,.T.);
#5415=EDGE_CURVE('',#4356,#4362,#2531,.T.);
#5416=EDGE_CURVE('',#4365,#4366,#2532,.T.);
#5417=EDGE_CURVE('',#4364,#4366,#2533,.T.);
#5418=EDGE_CURVE('',#4363,#4365,#2534,.T.);
#5419=EDGE_CURVE('',#4367,#4368,#2535,.T.);
#5420=EDGE_CURVE('',#4367,#4369,#2536,.T.);
#5421=EDGE_CURVE('',#4369,#4370,#2537,.T.);
#5422=EDGE_CURVE('',#4368,#4370,#2538,.T.);
#5423=EDGE_CURVE('',#4367,#4371,#2539,.T.);
#5424=EDGE_CURVE('',#4372,#4368,#2540,.T.);
#5425=EDGE_CURVE('',#4371,#4372,#2541,.T.);
#5426=EDGE_CURVE('',#4371,#4373,#2542,.T.);
#5427=EDGE_CURVE('',#4374,#4372,#2543,.T.);
#5428=EDGE_CURVE('',#4373,#4374,#2544,.T.);
#5429=EDGE_CURVE('',#4373,#4375,#3732,.T.);
#5430=EDGE_CURVE('',#4376,#4374,#3733,.T.);
#5431=EDGE_CURVE('',#4375,#4376,#2545,.T.);
#5432=EDGE_CURVE('',#4375,#4377,#2546,.T.);
#5433=EDGE_CURVE('',#4378,#4376,#2547,.T.);
#5434=EDGE_CURVE('',#4365,#4378,#2548,.T.);
#5435=EDGE_CURVE('',#4357,#4363,#2549,.T.);
#5436=EDGE_CURVE('',#4377,#4359,#2550,.T.);
#5437=EDGE_CURVE('',#4351,#4361,#2551,.T.);
#5438=EDGE_CURVE('',#4349,#4355,#2552,.T.);
#5439=EDGE_CURVE('',#4341,#4353,#2553,.T.);
#5440=EDGE_CURVE('',#4337,#4345,#2554,.T.);
#5441=EDGE_CURVE('',#4339,#4343,#2555,.T.);
#5442=EDGE_CURVE('',#4379,#4347,#2556,.T.);
#5443=EDGE_CURVE('',#4379,#4339,#2557,.T.);
#5444=EDGE_CURVE('',#4380,#4348,#2558,.T.);
#5445=EDGE_CURVE('',#4380,#4379,#2559,.T.);
#5446=EDGE_CURVE('',#4340,#4344,#2560,.T.);
#5447=EDGE_CURVE('',#4380,#4340,#2561,.T.);
#5448=EDGE_CURVE('',#4338,#4346,#2562,.T.);
#5449=EDGE_CURVE('',#4342,#4354,#2563,.T.);
#5450=EDGE_CURVE('',#4350,#4356,#2564,.T.);
#5451=EDGE_CURVE('',#4352,#4362,#2565,.T.);
#5452=EDGE_CURVE('',#4358,#4364,#2566,.T.);
#5453=EDGE_CURVE('',#4381,#4382,#2567,.T.);
#5454=EDGE_CURVE('',#4383,#4381,#2568,.T.);
#5455=EDGE_CURVE('',#4360,#4383,#2569,.T.);
#5456=EDGE_CURVE('',#4384,#4366,#2570,.T.);
#5457=EDGE_CURVE('',#4382,#4384,#2571,.T.);
#5458=EDGE_CURVE('',#4369,#4381,#3734,.T.);
#5459=EDGE_CURVE('',#4382,#4370,#3735,.T.);
#5460=EDGE_CURVE('',#4378,#4384,#2572,.T.);
#5461=EDGE_CURVE('',#4377,#4383,#2573,.T.);
#5462=EDGE_CURVE('',#4385,#4386,#2574,.T.);
#5463=EDGE_CURVE('',#4387,#4385,#3736,.T.);
#5464=EDGE_CURVE('',#4388,#4387,#2575,.T.);
#5465=EDGE_CURVE('',#4388,#4386,#3737,.T.);
#5466=EDGE_CURVE('',#4385,#4389,#2576,.T.);
#5467=EDGE_CURVE('',#4386,#4390,#2577,.T.);
#5468=EDGE_CURVE('',#4390,#4389,#2578,.T.);
#5469=EDGE_CURVE('',#4391,#4392,#2579,.T.);
#5470=EDGE_CURVE('',#4391,#4393,#3738,.T.);
#5471=EDGE_CURVE('',#4394,#4393,#2580,.T.);
#5472=EDGE_CURVE('',#4392,#4394,#3739,.T.);
#5473=EDGE_CURVE('',#4395,#4391,#2581,.T.);
#5474=EDGE_CURVE('',#4396,#4392,#2582,.T.);
#5475=EDGE_CURVE('',#4396,#4395,#2583,.T.);
#5476=EDGE_CURVE('',#4397,#4398,#2584,.T.);
#5477=EDGE_CURVE('',#4389,#4397,#3740,.T.);
#5478=EDGE_CURVE('',#4390,#4398,#3741,.T.);
#5479=EDGE_CURVE('',#4397,#4399,#2585,.T.);
#5480=EDGE_CURVE('',#4398,#4400,#2586,.T.);
#5481=EDGE_CURVE('',#4399,#4400,#2587,.T.);
#5482=EDGE_CURVE('',#4401,#4402,#2588,.T.);
#5483=EDGE_CURVE('',#4401,#4403,#3742,.T.);
#5484=EDGE_CURVE('',#4404,#4403,#2589,.T.);
#5485=EDGE_CURVE('',#4402,#4404,#3743,.T.);
#5486=EDGE_CURVE('',#4393,#4401,#2590,.T.);
#5487=EDGE_CURVE('',#4394,#4402,#2591,.T.);
#5488=EDGE_CURVE('',#4404,#4405,#2592,.T.);
#5489=EDGE_CURVE('',#4400,#4405,#2593,.T.);
#5490=EDGE_CURVE('',#4398,#4404,#2594,.T.);
#5491=EDGE_CURVE('',#4406,#4405,#2595,.T.);
#5492=EDGE_CURVE('',#4399,#4406,#2596,.T.);
#5493=EDGE_CURVE('',#4403,#4406,#2597,.T.);
#5494=EDGE_CURVE('',#4397,#4403,#2598,.T.);
#5495=EDGE_CURVE('',#4389,#4401,#2599,.T.);
#5496=EDGE_CURVE('',#4385,#4393,#2600,.T.);
#5497=EDGE_CURVE('',#4387,#4391,#2601,.T.);
#5498=EDGE_CURVE('',#4407,#4395,#2602,.T.);
#5499=EDGE_CURVE('',#4407,#4387,#2603,.T.);
#5500=EDGE_CURVE('',#4408,#4396,#2604,.T.);
#5501=EDGE_CURVE('',#4408,#4407,#2605,.T.);
#5502=EDGE_CURVE('',#4388,#4392,#2606,.T.);
#5503=EDGE_CURVE('',#4408,#4388,#2607,.T.);
#5504=EDGE_CURVE('',#4386,#4394,#2608,.T.);
#5505=EDGE_CURVE('',#4390,#4402,#2609,.T.);
#5506=EDGE_CURVE('',#4409,#4410,#3744,.T.);
#5507=EDGE_CURVE('',#4410,#4411,#153,.T.);
#5508=EDGE_CURVE('',#4412,#4411,#3745,.T.);
#5509=EDGE_CURVE('',#4412,#4409,#154,.T.);
#5510=EDGE_CURVE('',#4413,#4414,#276,.T.);
#5511=EDGE_CURVE('',#4412,#4414,#2610,.T.);
#5512=EDGE_CURVE('',#4413,#4411,#2611,.T.);
#5513=EDGE_CURVE('',#4415,#4416,#155,.T.);
#5514=EDGE_CURVE('',#4417,#4415,#277,.T.);
#5515=EDGE_CURVE('',#4418,#4417,#3746,.T.);
#5516=EDGE_CURVE('',#4419,#4418,#278,.T.);
#5517=EDGE_CURVE('',#4419,#4420,#156,.T.);
#5518=EDGE_CURVE('',#4421,#4420,#3747,.T.);
#5519=EDGE_CURVE('',#4421,#4422,#157,.T.);
#5520=EDGE_CURVE('',#4423,#4422,#279,.T.);
#5521=EDGE_CURVE('',#4424,#4423,#3748,.T.);
#5522=EDGE_CURVE('',#4425,#4424,#280,.T.);
#5523=EDGE_CURVE('',#4426,#4425,#3749,.T.);
#5524=EDGE_CURVE('',#4427,#4426,#281,.T.);
#5525=EDGE_CURVE('',#4428,#4427,#158,.T.);
#5526=EDGE_CURVE('',#4416,#4428,#3750,.T.);
#5527=EDGE_CURVE('',#4429,#4430,#159,.T.);
#5528=EDGE_CURVE('',#4431,#4429,#282,.T.);
#5529=EDGE_CURVE('',#4432,#4431,#160,.T.);
#5530=EDGE_CURVE('',#4433,#4432,#3751,.T.);
#5531=EDGE_CURVE('',#4434,#4433,#161,.F.);
#5532=EDGE_CURVE('',#4435,#4434,#3752,.T.);
#5533=EDGE_CURVE('',#4436,#4435,#162,.T.);
#5534=EDGE_CURVE('',#4430,#4436,#3753,.T.);
#5535=EDGE_CURVE('',#4437,#4438,#283,.T.);
#5536=EDGE_CURVE('',#4439,#4437,#3754,.T.);
#5537=EDGE_CURVE('',#4440,#4439,#284,.T.);
#5538=EDGE_CURVE('',#4438,#4440,#3755,.T.);
#5539=EDGE_CURVE('',#4441,#4442,#163,.T.);
#5540=EDGE_CURVE('',#4443,#4442,#3756,.T.);
#5541=EDGE_CURVE('',#4443,#4444,#164,.T.);
#5542=EDGE_CURVE('',#4445,#4444,#3757,.T.);
#5543=EDGE_CURVE('',#4445,#4446,#165,.T.);
#5544=EDGE_CURVE('',#4447,#4446,#3758,.T.);
#5545=EDGE_CURVE('',#4447,#4448,#166,.T.);
#5546=EDGE_CURVE('',#4449,#4448,#285,.T.);
#5547=EDGE_CURVE('',#4450,#4449,#3759,.T.);
#5548=EDGE_CURVE('',#4451,#4450,#3760,.T.);
#5549=EDGE_CURVE('',#4452,#4451,#167,.T.);
#5550=EDGE_CURVE('',#4453,#4452,#3761,.T.);
#5551=EDGE_CURVE('',#4454,#4453,#168,.F.);
#5552=EDGE_CURVE('',#4455,#4454,#286,.T.);
#5553=EDGE_CURVE('',#4456,#4455,#169,.T.);
#5554=EDGE_CURVE('',#4457,#4456,#3762,.T.);
#5555=EDGE_CURVE('',#4458,#4457,#170,.T.);
#5556=EDGE_CURVE('',#4459,#4458,#3763,.T.);
#5557=EDGE_CURVE('',#4460,#4459,#3764,.T.);
#5558=EDGE_CURVE('',#4441,#4460,#287,.T.);
#5559=EDGE_CURVE('',#4461,#4462,#171,.T.);
#5560=EDGE_CURVE('',#4463,#4461,#3765,.T.);
#5561=EDGE_CURVE('',#4464,#4463,#172,.T.);
#5562=EDGE_CURVE('',#4465,#4464,#3766,.T.);
#5563=EDGE_CURVE('',#4466,#4465,#173,.F.);
#5564=EDGE_CURVE('',#4467,#4466,#3767,.T.);
#5565=EDGE_CURVE('',#4468,#4467,#174,.T.);
#5566=EDGE_CURVE('',#4462,#4468,#3768,.T.);
#5567=EDGE_CURVE('',#4469,#4470,#175,.F.);
#5568=EDGE_CURVE('',#4471,#4469,#3769,.T.);
#5569=EDGE_CURVE('',#4472,#4471,#176,.T.);
#5570=EDGE_CURVE('',#4473,#4472,#3770,.T.);
#5571=EDGE_CURVE('',#4474,#4473,#177,.T.);
#5572=EDGE_CURVE('',#4475,#4474,#288,.T.);
#5573=EDGE_CURVE('',#4476,#4475,#3771,.T.);
#5574=EDGE_CURVE('',#4477,#4476,#289,.T.);
#5575=EDGE_CURVE('',#4477,#4478,#178,.T.);
#5576=EDGE_CURVE('',#4479,#4478,#3772,.T.);
#5577=EDGE_CURVE('',#4479,#4480,#179,.T.);
#5578=EDGE_CURVE('',#4481,#4480,#290,.T.);
#5579=EDGE_CURVE('',#4481,#4482,#180,.T.);
#5580=EDGE_CURVE('',#4483,#4482,#3773,.T.);
#5581=EDGE_CURVE('',#4484,#4483,#181,.T.);
#5582=EDGE_CURVE('',#4485,#4484,#3774,.T.);
#5583=EDGE_CURVE('',#4486,#4485,#182,.T.);
#5584=EDGE_CURVE('',#4487,#4486,#3775,.T.);
#5585=EDGE_CURVE('',#4488,#4487,#183,.F.);
#5586=EDGE_CURVE('',#4489,#4488,#291,.T.);
#5587=EDGE_CURVE('',#4490,#4489,#3776,.T.);
#5588=EDGE_CURVE('',#4491,#4490,#292,.T.);
#5589=EDGE_CURVE('',#4491,#4492,#184,.T.);
#5590=EDGE_CURVE('',#4493,#4492,#3777,.T.);
#5591=EDGE_CURVE('',#4493,#4494,#185,.T.);
#5592=EDGE_CURVE('',#4495,#4494,#293,.T.);
#5593=EDGE_CURVE('',#4495,#4496,#186,.T.);
#5594=EDGE_CURVE('',#4470,#4496,#3778,.T.);
#5595=EDGE_CURVE('',#4433,#4497,#2612,.T.);
#5596=EDGE_CURVE('',#4497,#4498,#187,.T.);
#5597=EDGE_CURVE('',#4434,#4498,#2613,.T.);
#5598=EDGE_CURVE('',#4499,#4500,#188,.F.);
#5599=EDGE_CURVE('',#4499,#4501,#2614,.T.);
#5600=EDGE_CURVE('',#4502,#4501,#189,.F.);
#5601=EDGE_CURVE('',#4500,#4502,#2615,.T.);
#5602=EDGE_CURVE('',#4453,#4503,#2616,.T.);
#5603=EDGE_CURVE('',#4503,#4504,#190,.T.);
#5604=EDGE_CURVE('',#4454,#4504,#2617,.T.);
#5605=EDGE_CURVE('',#4445,#4505,#2618,.T.);
#5606=EDGE_CURVE('',#4506,#4505,#191,.F.);
#5607=EDGE_CURVE('',#4446,#4506,#2619,.T.);
#5608=EDGE_CURVE('',#4507,#4508,#192,.F.);
#5609=EDGE_CURVE('',#4507,#4509,#2620,.T.);
#5610=EDGE_CURVE('',#4510,#4509,#193,.F.);
#5611=EDGE_CURVE('',#4508,#4510,#2621,.T.);
#5612=EDGE_CURVE('',#4465,#4511,#2622,.T.);
#5613=EDGE_CURVE('',#4511,#4512,#194,.T.);
#5614=EDGE_CURVE('',#4466,#4512,#2623,.T.);
#5615=EDGE_CURVE('',#4487,#4513,#2624,.T.);
#5616=EDGE_CURVE('',#4513,#4514,#195,.T.);
#5617=EDGE_CURVE('',#4488,#4514,#2625,.T.);
#5618=EDGE_CURVE('',#4481,#4515,#2626,.T.);
#5619=EDGE_CURVE('',#4516,#4515,#196,.F.);
#5620=EDGE_CURVE('',#4482,#4516,#2627,.T.);
#5621=EDGE_CURVE('',#4470,#4517,#2628,.T.);
#5622=EDGE_CURVE('',#4517,#4518,#197,.T.);
#5623=EDGE_CURVE('',#4469,#4518,#2629,.T.);
#5624=EDGE_CURVE('',#4491,#4519,#2630,.T.);
#5625=EDGE_CURVE('',#4520,#4519,#198,.F.);
#5626=EDGE_CURVE('',#4492,#4520,#2631,.T.);
#5627=EDGE_CURVE('',#4521,#4521,#3779,.T.);
#5628=EDGE_CURVE('',#4521,#4522,#2632,.T.);
#5629=EDGE_CURVE('',#4522,#4522,#3780,.T.);
#5630=EDGE_CURVE('',#4523,#4524,#3781,.T.);
#5631=EDGE_CURVE('',#4523,#4525,#199,.T.);
#5632=EDGE_CURVE('',#4525,#4526,#3782,.T.);
#5633=EDGE_CURVE('',#4526,#4524,#200,.T.);
#5634=EDGE_CURVE('',#4527,#4525,#2633,.T.);
#5635=EDGE_CURVE('',#4528,#4527,#294,.T.);
#5636=EDGE_CURVE('',#4526,#4528,#2634,.T.);
#5637=EDGE_CURVE('',#4529,#4529,#3783,.T.);
#5638=EDGE_CURVE('',#4529,#4530,#2635,.T.);
#5639=EDGE_CURVE('',#4530,#4530,#3784,.T.);
#5640=EDGE_CURVE('',#4531,#4531,#3785,.T.);
#5641=EDGE_CURVE('',#4531,#4532,#2636,.T.);
#5642=EDGE_CURVE('',#4532,#4532,#3786,.T.);
#5643=EDGE_CURVE('',#4533,#4413,#2637,.T.);
#5644=EDGE_CURVE('',#4534,#4533,#2638,.T.);
#5645=EDGE_CURVE('',#4534,#4528,#2639,.T.);
#5646=EDGE_CURVE('',#4527,#4535,#2640,.T.);
#5647=EDGE_CURVE('',#4536,#4535,#2641,.T.);
#5648=EDGE_CURVE('',#4414,#4536,#2642,.T.);
#5649=EDGE_CURVE('',#4537,#4538,#2643,.T.);
#5650=EDGE_CURVE('',#4538,#4539,#2644,.T.);
#5651=EDGE_CURVE('',#4539,#4540,#295,.T.);
#5652=EDGE_CURVE('',#4540,#4541,#2645,.T.);
#5653=EDGE_CURVE('',#4541,#4542,#296,.T.);
#5654=EDGE_CURVE('',#4542,#4543,#2646,.T.);
#5655=EDGE_CURVE('',#4543,#4544,#2647,.T.);
#5656=EDGE_CURVE('',#4545,#4544,#2648,.T.);
#5657=EDGE_CURVE('',#4546,#4545,#297,.T.);
#5658=EDGE_CURVE('',#4547,#4546,#2649,.T.);
#5659=EDGE_CURVE('',#4548,#4547,#298,.T.);
#5660=EDGE_CURVE('',#4537,#4548,#2650,.T.);
#5661=EDGE_CURVE('',#4543,#4534,#3787,.T.);
#5662=EDGE_CURVE('',#4544,#4533,#3788,.T.);
#5663=EDGE_CURVE('',#4535,#4538,#3789,.T.);
#5664=EDGE_CURVE('',#4536,#4537,#3790,.T.);
#5665=EDGE_CURVE('',#4540,#4523,#2651,.T.);
#5666=EDGE_CURVE('',#4541,#4524,#2652,.T.);
#5667=EDGE_CURVE('',#4542,#4526,#2653,.T.);
#5668=EDGE_CURVE('',#4539,#4525,#2654,.T.);
#5669=EDGE_CURVE('',#4546,#4410,#2655,.T.);
#5670=EDGE_CURVE('',#4545,#4411,#2656,.T.);
#5671=EDGE_CURVE('',#4548,#4412,#2657,.T.);
#5672=EDGE_CURVE('',#4547,#4409,#2658,.T.);
#5673=EDGE_CURVE('',#4493,#4549,#2659,.T.);
#5674=EDGE_CURVE('',#4550,#4549,#201,.T.);
#5675=EDGE_CURVE('',#4494,#4550,#2660,.T.);
#5676=EDGE_CURVE('',#4520,#4549,#3791,.T.);
#5677=EDGE_CURVE('',#4495,#4551,#2661,.T.);
#5678=EDGE_CURVE('',#4552,#4551,#202,.T.);
#5679=EDGE_CURVE('',#4496,#4552,#2662,.T.);
#5680=EDGE_CURVE('',#4550,#4551,#299,.T.);
#5681=EDGE_CURVE('',#4472,#4553,#2663,.T.);
#5682=EDGE_CURVE('',#4471,#4554,#2664,.T.);
#5683=EDGE_CURVE('',#4554,#4553,#203,.T.);
#5684=EDGE_CURVE('',#4474,#4555,#2665,.T.);
#5685=EDGE_CURVE('',#4473,#4556,#2666,.T.);
#5686=EDGE_CURVE('',#4556,#4555,#204,.T.);
#5687=EDGE_CURVE('',#4477,#4557,#2667,.T.);
#5688=EDGE_CURVE('',#4558,#4557,#205,.T.);
#5689=EDGE_CURVE('',#4478,#4558,#2668,.T.);
#5690=EDGE_CURVE('',#4475,#4559,#2669,.T.);
#5691=EDGE_CURVE('',#4555,#4559,#300,.T.);
#5692=EDGE_CURVE('',#4476,#4560,#2670,.T.);
#5693=EDGE_CURVE('',#4559,#4560,#3792,.T.);
#5694=EDGE_CURVE('',#4560,#4557,#301,.T.);
#5695=EDGE_CURVE('',#4479,#4561,#2671,.T.);
#5696=EDGE_CURVE('',#4562,#4561,#206,.T.);
#5697=EDGE_CURVE('',#4480,#4562,#2672,.T.);
#5698=EDGE_CURVE('',#4558,#4561,#3793,.T.);
#5699=EDGE_CURVE('',#4562,#4515,#302,.T.);
#5700=EDGE_CURVE('',#4484,#4563,#2673,.T.);
#5701=EDGE_CURVE('',#4483,#4564,#2674,.T.);
#5702=EDGE_CURVE('',#4564,#4563,#207,.T.);
#5703=EDGE_CURVE('',#4486,#4565,#2675,.T.);
#5704=EDGE_CURVE('',#4485,#4566,#2676,.T.);
#5705=EDGE_CURVE('',#4566,#4565,#208,.T.);
#5706=EDGE_CURVE('',#4489,#4567,#2677,.T.);
#5707=EDGE_CURVE('',#4514,#4567,#303,.T.);
#5708=EDGE_CURVE('',#4490,#4568,#2678,.T.);
#5709=EDGE_CURVE('',#4567,#4568,#3794,.T.);
#5710=EDGE_CURVE('',#4568,#4519,#304,.T.);
#5711=EDGE_CURVE('',#4565,#4513,#3795,.T.);
#5712=EDGE_CURVE('',#4563,#4566,#3796,.T.);
#5713=EDGE_CURVE('',#4516,#4564,#3797,.T.);
#5714=EDGE_CURVE('',#4553,#4556,#3798,.T.);
#5715=EDGE_CURVE('',#4518,#4554,#3799,.T.);
#5716=EDGE_CURVE('',#4552,#4517,#3800,.T.);
#5717=EDGE_CURVE('',#4468,#4569,#2679,.T.);
#5718=EDGE_CURVE('',#4467,#4570,#2680,.T.);
#5719=EDGE_CURVE('',#4570,#4569,#209,.T.);
#5720=EDGE_CURVE('',#4461,#4571,#2681,.T.);
#5721=EDGE_CURVE('',#4462,#4572,#2682,.T.);
#5722=EDGE_CURVE('',#4572,#4571,#210,.T.);
#5723=EDGE_CURVE('',#4464,#4573,#2683,.T.);
#5724=EDGE_CURVE('',#4463,#4574,#2684,.T.);
#5725=EDGE_CURVE('',#4574,#4573,#211,.T.);
#5726=EDGE_CURVE('',#4512,#4570,#3801,.T.);
#5727=EDGE_CURVE('',#4573,#4511,#3802,.T.);
#5728=EDGE_CURVE('',#4571,#4574,#3803,.T.);
#5729=EDGE_CURVE('',#4569,#4572,#3804,.T.);
#5730=EDGE_CURVE('',#4575,#4510,#3805,.T.);
#5731=EDGE_CURVE('',#4509,#4576,#3806,.T.);
#5732=EDGE_CURVE('',#4576,#4577,#212,.T.);
#5733=EDGE_CURVE('',#4577,#4578,#3807,.T.);
#5734=EDGE_CURVE('',#4578,#4579,#213,.T.);
#5735=EDGE_CURVE('',#4579,#4580,#3808,.T.);
#5736=EDGE_CURVE('',#4580,#4575,#214,.T.);
#5737=EDGE_CURVE('',#4581,#4575,#2685,.T.);
#5738=EDGE_CURVE('',#4508,#4581,#3809,.T.);
#5739=EDGE_CURVE('',#4582,#4507,#3810,.T.);
#5740=EDGE_CURVE('',#4582,#4576,#2686,.T.);
#5741=EDGE_CURVE('',#4583,#4582,#215,.T.);
#5742=EDGE_CURVE('',#4583,#4577,#2687,.T.);
#5743=EDGE_CURVE('',#4584,#4583,#3811,.T.);
#5744=EDGE_CURVE('',#4584,#4578,#2688,.T.);
#5745=EDGE_CURVE('',#4585,#4584,#216,.T.);
#5746=EDGE_CURVE('',#4585,#4579,#2689,.T.);
#5747=EDGE_CURVE('',#4586,#4585,#3812,.T.);
#5748=EDGE_CURVE('',#4586,#4580,#2690,.T.);
#5749=EDGE_CURVE('',#4581,#4586,#217,.T.);
#5750=EDGE_CURVE('',#4456,#4587,#2691,.T.);
#5751=EDGE_CURVE('',#4455,#4588,#2692,.T.);
#5752=EDGE_CURVE('',#4588,#4587,#218,.T.);
#5753=EDGE_CURVE('',#4458,#4589,#2693,.T.);
#5754=EDGE_CURVE('',#4457,#4590,#2694,.T.);
#5755=EDGE_CURVE('',#4590,#4589,#219,.T.);
#5756=EDGE_CURVE('',#4441,#4591,#2695,.T.);
#5757=EDGE_CURVE('',#4592,#4591,#220,.T.);
#5758=EDGE_CURVE('',#4442,#4592,#2696,.T.);
#5759=EDGE_CURVE('',#4459,#4593,#2697,.T.);
#5760=EDGE_CURVE('',#4589,#4593,#3813,.T.);
#5761=EDGE_CURVE('',#4460,#4594,#2698,.T.);
#5762=EDGE_CURVE('',#4593,#4594,#3814,.T.);
#5763=EDGE_CURVE('',#4594,#4591,#305,.T.);
#5764=EDGE_CURVE('',#4443,#4595,#2699,.T.);
#5765=EDGE_CURVE('',#4596,#4595,#221,.T.);
#5766=EDGE_CURVE('',#4444,#4596,#2700,.T.);
#5767=EDGE_CURVE('',#4592,#4595,#3815,.T.);
#5768=EDGE_CURVE('',#4596,#4505,#3816,.T.);
#5769=EDGE_CURVE('',#4447,#4597,#2701,.T.);
#5770=EDGE_CURVE('',#4598,#4597,#222,.T.);
#5771=EDGE_CURVE('',#4448,#4598,#2702,.T.);
#5772=EDGE_CURVE('',#4506,#4597,#3817,.T.);
#5773=EDGE_CURVE('',#4452,#4599,#2703,.T.);
#5774=EDGE_CURVE('',#4451,#4600,#2704,.T.);
#5775=EDGE_CURVE('',#4600,#4599,#223,.T.);
#5776=EDGE_CURVE('',#4504,#4588,#306,.T.);
#5777=EDGE_CURVE('',#4599,#4503,#3818,.T.);
#5778=EDGE_CURVE('',#4449,#4601,#2705,.T.);
#5779=EDGE_CURVE('',#4598,#4601,#307,.T.);
#5780=EDGE_CURVE('',#4450,#4602,#2706,.T.);
#5781=EDGE_CURVE('',#4601,#4602,#3819,.T.);
#5782=EDGE_CURVE('',#4602,#4600,#3820,.T.);
#5783=EDGE_CURVE('',#4587,#4590,#3821,.T.);
#5784=EDGE_CURVE('',#4428,#4603,#2707,.T.);
#5785=EDGE_CURVE('',#4427,#4604,#2708,.T.);
#5786=EDGE_CURVE('',#4604,#4603,#224,.T.);
#5787=EDGE_CURVE('',#4415,#4605,#2709,.T.);
#5788=EDGE_CURVE('',#4416,#4606,#2710,.T.);
#5789=EDGE_CURVE('',#4606,#4605,#225,.T.);
#5790=EDGE_CURVE('',#4419,#4607,#2711,.T.);
#5791=EDGE_CURVE('',#4608,#4607,#226,.T.);
#5792=EDGE_CURVE('',#4420,#4608,#2712,.T.);
#5793=EDGE_CURVE('',#4417,#4609,#2713,.T.);
#5794=EDGE_CURVE('',#4605,#4609,#308,.T.);
#5795=EDGE_CURVE('',#4418,#4610,#2714,.T.);
#5796=EDGE_CURVE('',#4609,#4610,#3822,.T.);
#5797=EDGE_CURVE('',#4610,#4607,#309,.T.);
#5798=EDGE_CURVE('',#4421,#4611,#2715,.T.);
#5799=EDGE_CURVE('',#4612,#4611,#227,.T.);
#5800=EDGE_CURVE('',#4422,#4612,#2716,.T.);
#5801=EDGE_CURVE('',#4608,#4611,#3823,.T.);
#5802=EDGE_CURVE('',#4425,#4613,#2717,.T.);
#5803=EDGE_CURVE('',#4424,#4614,#2718,.T.);
#5804=EDGE_CURVE('',#4614,#4613,#310,.T.);
#5805=EDGE_CURVE('',#4426,#4615,#2719,.T.);
#5806=EDGE_CURVE('',#4613,#4615,#3824,.T.);
#5807=EDGE_CURVE('',#4615,#4604,#311,.T.);
#5808=EDGE_CURVE('',#4423,#4616,#2720,.T.);
#5809=EDGE_CURVE('',#4612,#4616,#312,.T.);
#5810=EDGE_CURVE('',#4616,#4614,#3825,.T.);
#5811=EDGE_CURVE('',#4603,#4606,#3826,.T.);
#5812=EDGE_CURVE('',#4440,#4617,#2721,.T.);
#5813=EDGE_CURVE('',#4439,#4618,#2722,.T.);
#5814=EDGE_CURVE('',#4618,#4617,#313,.T.);
#5815=EDGE_CURVE('',#4438,#4619,#2723,.T.);
#5816=EDGE_CURVE('',#4617,#4619,#3827,.T.);
#5817=EDGE_CURVE('',#4437,#4620,#2724,.T.);
#5818=EDGE_CURVE('',#4619,#4620,#3828,.T.);
#5819=EDGE_CURVE('',#4620,#4618,#3829,.T.);
#5820=EDGE_CURVE('',#4501,#4621,#3830,.T.);
#5821=EDGE_CURVE('',#4622,#4499,#3831,.T.);
#5822=EDGE_CURVE('',#4622,#4621,#2725,.T.);
#5823=EDGE_CURVE('',#4621,#4623,#228,.T.);
#5824=EDGE_CURVE('',#4624,#4622,#229,.T.);
#5825=EDGE_CURVE('',#4624,#4623,#2726,.T.);
#5826=EDGE_CURVE('',#4623,#4625,#3832,.T.);
#5827=EDGE_CURVE('',#4626,#4624,#3833,.T.);
#5828=EDGE_CURVE('',#4626,#4625,#2727,.T.);
#5829=EDGE_CURVE('',#4625,#4627,#230,.T.);
#5830=EDGE_CURVE('',#4628,#4626,#231,.T.);
#5831=EDGE_CURVE('',#4628,#4627,#2728,.T.);
#5832=EDGE_CURVE('',#4627,#4629,#3834,.T.);
#5833=EDGE_CURVE('',#4630,#4628,#3835,.T.);
#5834=EDGE_CURVE('',#4630,#4629,#2729,.T.);
#5835=EDGE_CURVE('',#4629,#4631,#232,.T.);
#5836=EDGE_CURVE('',#4632,#4630,#233,.T.);
#5837=EDGE_CURVE('',#4632,#4631,#2730,.T.);
#5838=EDGE_CURVE('',#4631,#4502,#3836,.T.);
#5839=EDGE_CURVE('',#4500,#4632,#3837,.T.);
#5840=EDGE_CURVE('',#4498,#4633,#3838,.T.);
#5841=EDGE_CURVE('',#4634,#4497,#3839,.T.);
#5842=EDGE_CURVE('',#4635,#4634,#234,.T.);
#5843=EDGE_CURVE('',#4636,#4635,#314,.T.);
#5844=EDGE_CURVE('',#4637,#4636,#235,.T.);
#5845=EDGE_CURVE('',#4638,#4637,#3840,.T.);
#5846=EDGE_CURVE('',#4633,#4638,#236,.T.);
#5847=EDGE_CURVE('',#4432,#4634,#2731,.T.);
#5848=EDGE_CURVE('',#4431,#4635,#2732,.T.);
#5849=EDGE_CURVE('',#4429,#4636,#2733,.T.);
#5850=EDGE_CURVE('',#4430,#4637,#2734,.T.);
#5851=EDGE_CURVE('',#4436,#4638,#2735,.T.);
#5852=EDGE_CURVE('',#4435,#4633,#2736,.T.);
#5853=EDGE_CURVE('',#4639,#4639,#3841,.T.);
#5854=EDGE_CURVE('',#4639,#4640,#3842,.T.);
#5855=EDGE_CURVE('',#4640,#4640,#3843,.T.);
#5856=EDGE_CURVE('',#4641,#4641,#3844,.T.);
#5857=EDGE_CURVE('',#4641,#4639,#2737,.T.);
#5858=EDGE_CURVE('',#4642,#4642,#3845,.T.);
#5859=EDGE_CURVE('',#4642,#4641,#3846,.T.);
#5860=EDGE_CURVE('',#4643,#4644,#3847,.T.);
#5861=EDGE_CURVE('',#4644,#4643,#3848,.T.);
#5862=EDGE_CURVE('',#4644,#4645,#2738,.T.);
#5863=EDGE_CURVE('',#4645,#4645,#3849,.T.);
#5864=EDGE_CURVE('',#4643,#4646,#2739,.T.);
#5865=EDGE_CURVE('',#4646,#4646,#3850,.T.);
#5866=EDGE_CURVE('',#4647,#4648,#95,.T.);
#5867=EDGE_CURVE('',#4648,#4649,#96,.T.);
#5868=EDGE_CURVE('',#4649,#4647,#3851,.T.);
#5869=EDGE_CURVE('',#4650,#4651,#3852,.T.);
#5870=EDGE_CURVE('',#4652,#4650,#3853,.T.);
#5871=EDGE_CURVE('',#4647,#4652,#3854,.T.);
#5872=EDGE_CURVE('',#4653,#4649,#3855,.T.);
#5873=EDGE_CURVE('',#4651,#4653,#3856,.T.);
#5874=EDGE_CURVE('',#4651,#4654,#97,.T.);
#5875=EDGE_CURVE('',#4654,#4650,#98,.T.);
#5876=EDGE_CURVE('',#4650,#4655,#99,.T.);
#5877=EDGE_CURVE('',#4655,#4652,#100,.T.);
#5878=EDGE_CURVE('',#4652,#4656,#101,.T.);
#5879=EDGE_CURVE('',#4656,#4647,#102,.T.);
#5880=EDGE_CURVE('',#4649,#4657,#103,.T.);
#5881=EDGE_CURVE('',#4657,#4653,#104,.T.);
#5882=EDGE_CURVE('',#4653,#4658,#105,.T.);
#5883=EDGE_CURVE('',#4658,#4651,#106,.T.);
#5884=EDGE_CURVE('',#4659,#4656,#2740,.T.);
#5885=EDGE_CURVE('',#4660,#4659,#2741,.T.);
#5886=EDGE_CURVE('',#4660,#4648,#2742,.T.);
#5887=EDGE_CURVE('',#4661,#4655,#2743,.T.);
#5888=EDGE_CURVE('',#4659,#4661,#2744,.T.);
#5889=EDGE_CURVE('',#4662,#4654,#2745,.T.);
#5890=EDGE_CURVE('',#4661,#4662,#2746,.T.);
#5891=EDGE_CURVE('',#4663,#4658,#2747,.T.);
#5892=EDGE_CURVE('',#4662,#4663,#2748,.T.);
#5893=EDGE_CURVE('',#4664,#4657,#2749,.T.);
#5894=EDGE_CURVE('',#4663,#4664,#2750,.T.);
#5895=EDGE_CURVE('',#4664,#4660,#2751,.T.);
#5896=EDGE_CURVE('',#4665,#4665,#3857,.T.);
#5897=EDGE_CURVE('',#4665,#4666,#2752,.T.);
#5898=EDGE_CURVE('',#4666,#4666,#3858,.T.);
#5899=EDGE_CURVE('',#4667,#4667,#3859,.T.);
#5900=EDGE_CURVE('',#4667,#4668,#3860,.T.);
#5901=EDGE_CURVE('',#4668,#4669,#3861,.T.);
#5902=EDGE_CURVE('',#4669,#4668,#3862,.T.);
#5903=EDGE_CURVE('',#4670,#4671,#3863,.T.);
#5904=EDGE_CURVE('',#4671,#4670,#3864,.T.);
#5905=EDGE_CURVE('',#4671,#4669,#2753,.T.);
#5906=EDGE_CURVE('',#4672,#4672,#3865,.T.);
#5907=EDGE_CURVE('',#4672,#4673,#2754,.T.);
#5908=EDGE_CURVE('',#4673,#4673,#3866,.T.);
#5909=EDGE_CURVE('',#4673,#4674,#3867,.T.);
#5910=EDGE_CURVE('',#4674,#4674,#3868,.T.);
#5911=EDGE_CURVE('',#4675,#4675,#3869,.T.);
#5912=EDGE_CURVE('',#4675,#4676,#2755,.T.);
#5913=EDGE_CURVE('',#4676,#4676,#3870,.T.);
#5914=EDGE_CURVE('',#4677,#4677,#3871,.T.);
#5915=EDGE_CURVE('',#4677,#4678,#3872,.T.);
#5916=EDGE_CURVE('',#4678,#4678,#3873,.T.);
#5917=EDGE_CURVE('',#4678,#4679,#3874,.T.);
#5918=EDGE_CURVE('',#4679,#4679,#3875,.T.);
#5919=EDGE_CURVE('',#4680,#4680,#3876,.T.);
#5920=EDGE_CURVE('',#4680,#4681,#3877,.T.);
#5921=EDGE_CURVE('',#4681,#4682,#3878,.T.);
#5922=EDGE_CURVE('',#4682,#4681,#3879,.T.);
#5923=EDGE_CURVE('',#4683,#4684,#3880,.T.);
#5924=EDGE_CURVE('',#4684,#4682,#2756,.T.);
#5925=EDGE_CURVE('',#4684,#4683,#3881,.T.);
#5926=EDGE_CURVE('',#4683,#4685,#3882,.T.);
#5927=EDGE_CURVE('',#4685,#4685,#3883,.T.);
#5928=EDGE_CURVE('',#4670,#4672,#3884,.T.);
#5929=EDGE_CURVE('',#4686,#4686,#3885,.T.);
#5930=EDGE_CURVE('',#4686,#4687,#2757,.T.);
#5931=EDGE_CURVE('',#4687,#4688,#3886,.T.);
#5932=EDGE_CURVE('',#4688,#4689,#3887,.T.);
#5933=EDGE_CURVE('',#4689,#4690,#3888,.T.);
#5934=EDGE_CURVE('',#4690,#4691,#3889,.T.);
#5935=EDGE_CURVE('',#4691,#4692,#3890,.T.);
#5936=EDGE_CURVE('',#4692,#4687,#3891,.T.);
#5937=EDGE_CURVE('',#4693,#4694,#3892,.T.);
#5938=EDGE_CURVE('',#4694,#4695,#2758,.T.);
#5939=EDGE_CURVE('',#4695,#4695,#3893,.T.);
#5940=EDGE_CURVE('',#4694,#4693,#3894,.T.);
#5941=EDGE_CURVE('',#4693,#4696,#2759,.T.);
#5942=EDGE_CURVE('',#4696,#4696,#3895,.T.);
#5943=EDGE_CURVE('',#4696,#4697,#2760,.T.);
#5944=EDGE_CURVE('',#4697,#4697,#3896,.T.);
#5945=EDGE_CURVE('',#4698,#4699,#107,.T.);
#5946=EDGE_CURVE('',#4699,#4700,#108,.T.);
#5947=EDGE_CURVE('',#4700,#4698,#3897,.T.);
#5948=EDGE_CURVE('',#4701,#4702,#3898,.T.);
#5949=EDGE_CURVE('',#4703,#4701,#3899,.T.);
#5950=EDGE_CURVE('',#4698,#4703,#3900,.T.);
#5951=EDGE_CURVE('',#4704,#4700,#3901,.T.);
#5952=EDGE_CURVE('',#4702,#4704,#3902,.T.);
#5953=EDGE_CURVE('',#4702,#4705,#109,.T.);
#5954=EDGE_CURVE('',#4705,#4701,#110,.T.);
#5955=EDGE_CURVE('',#4701,#4706,#111,.T.);
#5956=EDGE_CURVE('',#4706,#4703,#112,.T.);
#5957=EDGE_CURVE('',#4703,#4707,#113,.T.);
#5958=EDGE_CURVE('',#4707,#4698,#114,.T.);
#5959=EDGE_CURVE('',#4700,#4708,#115,.T.);
#5960=EDGE_CURVE('',#4708,#4704,#116,.T.);
#5961=EDGE_CURVE('',#4704,#4709,#117,.T.);
#5962=EDGE_CURVE('',#4709,#4702,#118,.T.);
#5963=EDGE_CURVE('',#4710,#4707,#2761,.T.);
#5964=EDGE_CURVE('',#4688,#4710,#2762,.T.);
#5965=EDGE_CURVE('',#4711,#4688,#2763,.T.);
#5966=EDGE_CURVE('',#4711,#4699,#2764,.T.);
#5967=EDGE_CURVE('',#4712,#4706,#2765,.T.);
#5968=EDGE_CURVE('',#4689,#4712,#2766,.T.);
#5969=EDGE_CURVE('',#4710,#4689,#2767,.T.);
#5970=EDGE_CURVE('',#4713,#4705,#2768,.T.);
#5971=EDGE_CURVE('',#4690,#4713,#2769,.T.);
#5972=EDGE_CURVE('',#4712,#4690,#2770,.T.);
#5973=EDGE_CURVE('',#4714,#4709,#2771,.T.);
#5974=EDGE_CURVE('',#4691,#4714,#2772,.T.);
#5975=EDGE_CURVE('',#4713,#4691,#2773,.T.);
#5976=EDGE_CURVE('',#4715,#4708,#2774,.T.);
#5977=EDGE_CURVE('',#4692,#4715,#2775,.T.);
#5978=EDGE_CURVE('',#4714,#4692,#2776,.T.);
#5979=EDGE_CURVE('',#4687,#4711,#2777,.T.);
#5980=EDGE_CURVE('',#4715,#4687,#2778,.T.);
#5981=EDGE_CURVE('',#4716,#4717,#3903,.T.);
#5982=EDGE_CURVE('',#4718,#4716,#3904,.T.);
#5983=EDGE_CURVE('',#4719,#4718,#3905,.T.);
#5984=EDGE_CURVE('',#4719,#4720,#3906,.T.);
#5985=EDGE_CURVE('',#4717,#4720,#3907,.T.);
#5986=EDGE_CURVE('',#4721,#4721,#3908,.T.);
#5987=EDGE_CURVE('',#4721,#4718,#2779,.T.);
#5988=EDGE_CURVE('',#4716,#4722,#2780,.T.);
#5989=EDGE_CURVE('',#4722,#4723,#3909,.T.);
#5990=EDGE_CURVE('',#4719,#4723,#2781,.T.);
#5991=EDGE_CURVE('',#4724,#4724,#3910,.T.);
#5992=EDGE_CURVE('',#4724,#4725,#2782,.T.);
#5993=EDGE_CURVE('',#4725,#4725,#3911,.T.);
#5994=EDGE_CURVE('',#4726,#4726,#3912,.T.);
#5995=EDGE_CURVE('',#4726,#4724,#2783,.T.);
#5996=EDGE_CURVE('',#4727,#4727,#3913,.T.);
#5997=EDGE_CURVE('',#4727,#4728,#3914,.T.);
#5998=EDGE_CURVE('',#4728,#4728,#3915,.T.);
#5999=EDGE_CURVE('',#4729,#4729,#3916,.T.);
#6000=EDGE_CURVE('',#4729,#4727,#2784,.T.);
#6001=EDGE_CURVE('',#4730,#4730,#3917,.T.);
#6002=EDGE_CURVE('',#4730,#4721,#2785,.T.);
#6003=EDGE_CURVE('',#4731,#4731,#3918,.T.);
#6004=EDGE_CURVE('',#4731,#4730,#3919,.T.);
#6005=EDGE_CURVE('',#4732,#4733,#3920,.T.);
#6006=EDGE_CURVE('',#4733,#4732,#3921,.T.);
#6007=EDGE_CURVE('',#4733,#4734,#2786,.T.);
#6008=EDGE_CURVE('',#4734,#4734,#3922,.T.);
#6009=EDGE_CURVE('',#4732,#4735,#2787,.T.);
#6010=EDGE_CURVE('',#4735,#4735,#3923,.T.);
#6011=EDGE_CURVE('',#4736,#4736,#3924,.T.);
#6012=EDGE_CURVE('',#4736,#4737,#3925,.T.);
#6013=EDGE_CURVE('',#4737,#4737,#3926,.T.);
#6014=EDGE_CURVE('',#4738,#4738,#3927,.T.);
#6015=EDGE_CURVE('',#4738,#4736,#2788,.T.);
#6016=EDGE_CURVE('',#4739,#4739,#3928,.T.);
#6017=EDGE_CURVE('',#4739,#4738,#2789,.T.);
#6018=EDGE_CURVE('',#4722,#4717,#2790,.T.);
#6019=EDGE_CURVE('',#4723,#4720,#2791,.T.);
#6020=EDGE_CURVE('',#4740,#4740,#3929,.T.);
#6021=EDGE_CURVE('',#4740,#4741,#3930,.T.);
#6022=EDGE_CURVE('',#4741,#4741,#3931,.T.);
#6023=EDGE_CURVE('',#4742,#4743,#3932,.T.);
#6024=EDGE_CURVE('',#4743,#4742,#3933,.T.);
#6025=EDGE_CURVE('',#4743,#4740,#3934,.T.);
#6026=EDGE_CURVE('',#4744,#4744,#3935,.T.);
#6027=EDGE_CURVE('',#4744,#4745,#2792,.T.);
#6028=EDGE_CURVE('',#4745,#4745,#3936,.T.);
#6029=EDGE_CURVE('',#4746,#4746,#3937,.T.);
#6030=EDGE_CURVE('',#4746,#4747,#3938,.T.);
#6031=EDGE_CURVE('',#4747,#4748,#3939,.T.);
#6032=EDGE_CURVE('',#4748,#4747,#3940,.T.);
#6033=EDGE_CURVE('',#4742,#4748,#2793,.T.);
#6034=EDGE_CURVE('',#4741,#4749,#3941,.T.);
#6035=EDGE_CURVE('',#4749,#4749,#3942,.T.);
#6036=EDGE_CURVE('',#4749,#4750,#3943,.T.);
#6037=EDGE_CURVE('',#4750,#4750,#3944,.T.);
#6038=EDGE_CURVE('',#4751,#4751,#3945,.T.);
#6039=EDGE_CURVE('',#4751,#4752,#3946,.T.);
#6040=EDGE_CURVE('',#4752,#4752,#3947,.T.);
#6041=EDGE_CURVE('',#4752,#4753,#3948,.T.);
#6042=EDGE_CURVE('',#4753,#4754,#3949,.T.);
#6043=EDGE_CURVE('',#4754,#4753,#3950,.T.);
#6044=EDGE_CURVE('',#4755,#4756,#3951,.T.);
#6045=EDGE_CURVE('',#4756,#4754,#2794,.T.);
#6046=EDGE_CURVE('',#4756,#4755,#3952,.T.);
#6047=EDGE_CURVE('',#4755,#4757,#3953,.T.);
#6048=EDGE_CURVE('',#4757,#4757,#3954,.T.);
#6049=EDGE_CURVE('',#4758,#4759,#2795,.T.);
#6050=EDGE_CURVE('',#4760,#4759,#2796,.T.);
#6051=EDGE_CURVE('',#4760,#4761,#2797,.T.);
#6052=EDGE_CURVE('',#4761,#4758,#2798,.T.);
#6053=EDGE_CURVE('',#4759,#4762,#2799,.T.);
#6054=EDGE_CURVE('',#4763,#4762,#2800,.T.);
#6055=EDGE_CURVE('',#4763,#4760,#2801,.T.);
#6056=EDGE_CURVE('',#4762,#4764,#2802,.T.);
#6057=EDGE_CURVE('',#4765,#4764,#2803,.T.);
#6058=EDGE_CURVE('',#4765,#4763,#2804,.T.);
#6059=EDGE_CURVE('',#4764,#4766,#2805,.T.);
#6060=EDGE_CURVE('',#4767,#4766,#2806,.T.);
#6061=EDGE_CURVE('',#4767,#4765,#2807,.T.);
#6062=EDGE_CURVE('',#4766,#4768,#2808,.T.);
#6063=EDGE_CURVE('',#4769,#4768,#2809,.T.);
#6064=EDGE_CURVE('',#4769,#4767,#2810,.T.);
#6065=EDGE_CURVE('',#4768,#4770,#2811,.T.);
#6066=EDGE_CURVE('',#4771,#4770,#2812,.T.);
#6067=EDGE_CURVE('',#4771,#4769,#2813,.T.);
#6068=EDGE_CURVE('',#4770,#4772,#2814,.T.);
#6069=EDGE_CURVE('',#4773,#4772,#2815,.T.);
#6070=EDGE_CURVE('',#4773,#4771,#2816,.T.);
#6071=EDGE_CURVE('',#4772,#4758,#2817,.T.);
#6072=EDGE_CURVE('',#4761,#4773,#2818,.T.);
#6073=EDGE_CURVE('',#4774,#4774,#3955,.T.);
#6074=EDGE_CURVE('',#4774,#4775,#2819,.T.);
#6075=EDGE_CURVE('',#4775,#4775,#3956,.T.);
#6076=EDGE_CURVE('',#4776,#4776,#3957,.T.);
#6077=EDGE_CURVE('',#4776,#4777,#2820,.T.);
#6078=EDGE_CURVE('',#4777,#4777,#3958,.T.);
#6079=EDGE_CURVE('',#4778,#4778,#3959,.T.);
#6080=EDGE_CURVE('',#4778,#4779,#2821,.T.);
#6081=EDGE_CURVE('',#4779,#4779,#3960,.T.);
#6082=EDGE_CURVE('',#4780,#4780,#3961,.T.);
#6083=EDGE_CURVE('',#4780,#4781,#3962,.T.);
#6084=EDGE_CURVE('',#4781,#4781,#3963,.T.);
#6085=EDGE_CURVE('',#4782,#4782,#3964,.T.);
#6086=EDGE_CURVE('',#4782,#4780,#2822,.T.);
#6087=EDGE_CURVE('',#4783,#4783,#3965,.T.);
#6088=EDGE_CURVE('',#4783,#4782,#3966,.T.);
#6089=EDGE_CURVE('',#4784,#4784,#3967,.T.);
#6090=EDGE_CURVE('',#4784,#4785,#2823,.T.);
#6091=EDGE_CURVE('',#4785,#4785,#3968,.T.);
#6092=EDGE_CURVE('',#4786,#4786,#3969,.T.);
#6093=EDGE_CURVE('',#4786,#4787,#2824,.T.);
#6094=EDGE_CURVE('',#4787,#4787,#3970,.T.);
#6095=EDGE_CURVE('',#4788,#4788,#3971,.T.);
#6096=EDGE_CURVE('',#4788,#4789,#2825,.T.);
#6097=EDGE_CURVE('',#4789,#4789,#3972,.T.);
#6098=EDGE_CURVE('',#4790,#4790,#3973,.T.);
#6099=EDGE_CURVE('',#4790,#4791,#2826,.T.);
#6100=EDGE_CURVE('',#4791,#4791,#3974,.T.);
#6101=EDGE_CURVE('',#4792,#4792,#3975,.T.);
#6102=EDGE_CURVE('',#4792,#4793,#2827,.T.);
#6103=EDGE_CURVE('',#4793,#4793,#3976,.T.);
#6104=EDGE_CURVE('',#4794,#4794,#3977,.T.);
#6105=EDGE_CURVE('',#4794,#4795,#3978,.T.);
#6106=EDGE_CURVE('',#4795,#4795,#3979,.T.);
#6107=EDGE_CURVE('',#4795,#4796,#2828,.T.);
#6108=EDGE_CURVE('',#4796,#4796,#3980,.T.);
#6109=EDGE_CURVE('',#4796,#4797,#3981,.T.);
#6110=EDGE_CURVE('',#4797,#4797,#3982,.T.);
#6111=EDGE_CURVE('',#4798,#4798,#3983,.T.);
#6112=EDGE_CURVE('',#4798,#4799,#2829,.T.);
#6113=EDGE_CURVE('',#4799,#4799,#3984,.T.);
#6114=EDGE_CURVE('',#4800,#4800,#3985,.T.);
#6115=EDGE_CURVE('',#4800,#4801,#3986,.T.);
#6116=EDGE_CURVE('',#4801,#4802,#3987,.T.);
#6117=EDGE_CURVE('',#4802,#4801,#3988,.T.);
#6118=EDGE_CURVE('',#4803,#4804,#3989,.T.);
#6119=EDGE_CURVE('',#4804,#4802,#2830,.T.);
#6120=EDGE_CURVE('',#4804,#4803,#3990,.T.);
#6121=EDGE_CURVE('',#4803,#4805,#3991,.T.);
#6122=EDGE_CURVE('',#4805,#4806,#3992,.T.);
#6123=EDGE_CURVE('',#4806,#4805,#3993,.T.);
#6124=EDGE_CURVE('',#4807,#4808,#3994,.T.);
#6125=EDGE_CURVE('',#4808,#4806,#2831,.T.);
#6126=EDGE_CURVE('',#4808,#4807,#3995,.T.);
#6127=EDGE_CURVE('',#4807,#4809,#2832,.T.);
#6128=EDGE_CURVE('',#4809,#4809,#3996,.T.);
#6129=EDGE_CURVE('',#4809,#4810,#3997,.T.);
#6130=EDGE_CURVE('',#4810,#4810,#3998,.T.);
#6131=EDGE_CURVE('',#4810,#4811,#2833,.T.);
#6132=EDGE_CURVE('',#4811,#4811,#3999,.T.);
#6133=EDGE_CURVE('',#4811,#4812,#4000,.T.);
#6134=EDGE_CURVE('',#4812,#4812,#4001,.T.);
#6135=EDGE_CURVE('',#4813,#4813,#4002,.T.);
#6136=EDGE_CURVE('',#4813,#4814,#2834,.T.);
#6137=EDGE_CURVE('',#4814,#4814,#4003,.T.);
#6138=EDGE_CURVE('',#4815,#4815,#4004,.T.);
#6139=EDGE_CURVE('',#4815,#4816,#2835,.T.);
#6140=EDGE_CURVE('',#4816,#4816,#4005,.T.);
#6141=EDGE_CURVE('',#4817,#4818,#4006,.T.);
#6142=EDGE_CURVE('',#4818,#4819,#2836,.T.);
#6143=EDGE_CURVE('',#4819,#4819,#4007,.T.);
#6144=EDGE_CURVE('',#4818,#4817,#4008,.T.);
#6145=EDGE_CURVE('',#4817,#4820,#2837,.T.);
#6146=EDGE_CURVE('',#4820,#4820,#4009,.T.);
#6147=EDGE_CURVE('',#4820,#4821,#2838,.T.);
#6148=EDGE_CURVE('',#4821,#4821,#4010,.T.);
#6149=EDGE_CURVE('',#4822,#4822,#4011,.T.);
#6150=EDGE_CURVE('',#4822,#4823,#2839,.T.);
#6151=EDGE_CURVE('',#4823,#4823,#4012,.T.);
#6152=ORIENTED_EDGE('',*,*,#4824,.T.);
#6153=ORIENTED_EDGE('',*,*,#4825,.T.);
#6154=ORIENTED_EDGE('',*,*,#4826,.T.);
#6155=ORIENTED_EDGE('',*,*,#4825,.F.);
#6156=ORIENTED_EDGE('',*,*,#4827,.T.);
#6157=ORIENTED_EDGE('',*,*,#4828,.T.);
#6158=ORIENTED_EDGE('',*,*,#4829,.T.);
#6159=ORIENTED_EDGE('',*,*,#4828,.F.);
#6160=ORIENTED_EDGE('',*,*,#4830,.F.);
#6161=ORIENTED_EDGE('',*,*,#4831,.T.);
#6162=ORIENTED_EDGE('',*,*,#4832,.T.);
#6163=ORIENTED_EDGE('',*,*,#4831,.F.);
#6164=ORIENTED_EDGE('',*,*,#4833,.F.);
#6165=ORIENTED_EDGE('',*,*,#4834,.T.);
#6166=ORIENTED_EDGE('',*,*,#4835,.T.);
#6167=ORIENTED_EDGE('',*,*,#4834,.F.);
#6168=ORIENTED_EDGE('',*,*,#4836,.F.);
#6169=ORIENTED_EDGE('',*,*,#4837,.T.);
#6170=ORIENTED_EDGE('',*,*,#4838,.T.);
#6171=ORIENTED_EDGE('',*,*,#4837,.F.);
#6172=ORIENTED_EDGE('',*,*,#4839,.F.);
#6173=ORIENTED_EDGE('',*,*,#4840,.T.);
#6174=ORIENTED_EDGE('',*,*,#4841,.T.);
#6175=ORIENTED_EDGE('',*,*,#4840,.F.);
#6176=ORIENTED_EDGE('',*,*,#4842,.F.);
#6177=ORIENTED_EDGE('',*,*,#4843,.T.);
#6178=ORIENTED_EDGE('',*,*,#4844,.T.);
#6179=ORIENTED_EDGE('',*,*,#4843,.F.);
#6180=ORIENTED_EDGE('',*,*,#4845,.F.);
#6181=ORIENTED_EDGE('',*,*,#4846,.T.);
#6182=ORIENTED_EDGE('',*,*,#4847,.T.);
#6183=ORIENTED_EDGE('',*,*,#4846,.F.);
#6184=ORIENTED_EDGE('',*,*,#4848,.F.);
#6185=ORIENTED_EDGE('',*,*,#4849,.T.);
#6186=ORIENTED_EDGE('',*,*,#4850,.T.);
#6187=ORIENTED_EDGE('',*,*,#4849,.F.);
#6188=ORIENTED_EDGE('',*,*,#4851,.F.);
#6189=ORIENTED_EDGE('',*,*,#4852,.T.);
#6190=ORIENTED_EDGE('',*,*,#4853,.T.);
#6191=ORIENTED_EDGE('',*,*,#4852,.F.);
#6192=ORIENTED_EDGE('',*,*,#4854,.F.);
#6193=ORIENTED_EDGE('',*,*,#4855,.T.);
#6194=ORIENTED_EDGE('',*,*,#4856,.T.);
#6195=ORIENTED_EDGE('',*,*,#4855,.F.);
#6196=ORIENTED_EDGE('',*,*,#4857,.T.);
#6197=ORIENTED_EDGE('',*,*,#4858,.T.);
#6198=ORIENTED_EDGE('',*,*,#4859,.F.);
#6199=ORIENTED_EDGE('',*,*,#4860,.T.);
#6200=ORIENTED_EDGE('',*,*,#4861,.F.);
#6201=ORIENTED_EDGE('',*,*,#4862,.T.);
#6202=ORIENTED_EDGE('',*,*,#4863,.T.);
#6203=ORIENTED_EDGE('',*,*,#4864,.T.);
#6204=ORIENTED_EDGE('',*,*,#4865,.T.);
#6205=ORIENTED_EDGE('',*,*,#4866,.T.);
#6206=ORIENTED_EDGE('',*,*,#4867,.F.);
#6207=ORIENTED_EDGE('',*,*,#4868,.T.);
#6208=ORIENTED_EDGE('',*,*,#4869,.F.);
#6209=ORIENTED_EDGE('',*,*,#4870,.F.);
#6210=ORIENTED_EDGE('',*,*,#4871,.F.);
#6211=ORIENTED_EDGE('',*,*,#4872,.T.);
#6212=ORIENTED_EDGE('',*,*,#4873,.T.);
#6213=ORIENTED_EDGE('',*,*,#4874,.T.);
#6214=ORIENTED_EDGE('',*,*,#4875,.F.);
#6215=ORIENTED_EDGE('',*,*,#4876,.T.);
#6216=ORIENTED_EDGE('',*,*,#4877,.T.);
#6217=ORIENTED_EDGE('',*,*,#4878,.T.);
#6218=ORIENTED_EDGE('',*,*,#4879,.F.);
#6219=ORIENTED_EDGE('',*,*,#4880,.T.);
#6220=ORIENTED_EDGE('',*,*,#4881,.F.);
#6221=ORIENTED_EDGE('',*,*,#4882,.F.);
#6222=ORIENTED_EDGE('',*,*,#4883,.F.);
#6223=ORIENTED_EDGE('',*,*,#4884,.T.);
#6224=ORIENTED_EDGE('',*,*,#4885,.F.);
#6225=ORIENTED_EDGE('',*,*,#4881,.T.);
#6226=ORIENTED_EDGE('',*,*,#4886,.T.);
#6227=ORIENTED_EDGE('',*,*,#4887,.T.);
#6228=ORIENTED_EDGE('',*,*,#4888,.F.);
#6229=ORIENTED_EDGE('',*,*,#4889,.T.);
#6230=ORIENTED_EDGE('',*,*,#4890,.F.);
#6231=ORIENTED_EDGE('',*,*,#4891,.F.);
#6232=ORIENTED_EDGE('',*,*,#4892,.T.);
#6233=ORIENTED_EDGE('',*,*,#4888,.T.);
#6234=ORIENTED_EDGE('',*,*,#4893,.F.);
#6235=ORIENTED_EDGE('',*,*,#4894,.T.);
#6236=ORIENTED_EDGE('',*,*,#4895,.F.);
#6237=ORIENTED_EDGE('',*,*,#4896,.F.);
#6238=ORIENTED_EDGE('',*,*,#4887,.F.);
#6239=ORIENTED_EDGE('',*,*,#4897,.T.);
#6240=ORIENTED_EDGE('',*,*,#4898,.F.);
#6241=ORIENTED_EDGE('',*,*,#4895,.T.);
#6242=ORIENTED_EDGE('',*,*,#4899,.T.);
#6243=ORIENTED_EDGE('',*,*,#4900,.T.);
#6244=ORIENTED_EDGE('',*,*,#4901,.F.);
#6245=ORIENTED_EDGE('',*,*,#4902,.T.);
#6246=ORIENTED_EDGE('',*,*,#4903,.F.);
#6247=ORIENTED_EDGE('',*,*,#4904,.F.);
#6248=ORIENTED_EDGE('',*,*,#4905,.T.);
#6249=ORIENTED_EDGE('',*,*,#4901,.T.);
#6250=ORIENTED_EDGE('',*,*,#4906,.F.);
#6251=ORIENTED_EDGE('',*,*,#4890,.T.);
#6252=ORIENTED_EDGE('',*,*,#4876,.F.);
#6253=ORIENTED_EDGE('',*,*,#4907,.F.);
#6254=ORIENTED_EDGE('',*,*,#4900,.F.);
#6255=ORIENTED_EDGE('',*,*,#4908,.T.);
#6256=ORIENTED_EDGE('',*,*,#4909,.F.);
#6257=ORIENTED_EDGE('',*,*,#4910,.T.);
#6258=ORIENTED_EDGE('',*,*,#4864,.F.);
#6259=ORIENTED_EDGE('',*,*,#4911,.F.);
#6260=ORIENTED_EDGE('',*,*,#4912,.T.);
#6261=ORIENTED_EDGE('',*,*,#4909,.T.);
#6262=ORIENTED_EDGE('',*,*,#4913,.F.);
#6263=ORIENTED_EDGE('',*,*,#4903,.T.);
#6264=ORIENTED_EDGE('',*,*,#4914,.F.);
#6265=ORIENTED_EDGE('',*,*,#4915,.F.);
#6266=ORIENTED_EDGE('',*,*,#4880,.F.);
#6267=ORIENTED_EDGE('',*,*,#4916,.T.);
#6268=ORIENTED_EDGE('',*,*,#4917,.F.);
#6269=ORIENTED_EDGE('',*,*,#4914,.T.);
#6270=ORIENTED_EDGE('',*,*,#4918,.T.);
#6271=ORIENTED_EDGE('',*,*,#4919,.T.);
#6272=ORIENTED_EDGE('',*,*,#4860,.F.);
#6273=ORIENTED_EDGE('',*,*,#4920,.T.);
#6274=ORIENTED_EDGE('',*,*,#4921,.F.);
#6275=ORIENTED_EDGE('',*,*,#4922,.F.);
#6276=ORIENTED_EDGE('',*,*,#4923,.F.);
#6277=ORIENTED_EDGE('',*,*,#4924,.F.);
#6278=ORIENTED_EDGE('',*,*,#4919,.F.);
#6279=ORIENTED_EDGE('',*,*,#4925,.T.);
#6280=ORIENTED_EDGE('',*,*,#4926,.F.);
#6281=ORIENTED_EDGE('',*,*,#4923,.T.);
#6282=ORIENTED_EDGE('',*,*,#4927,.T.);
#6283=ORIENTED_EDGE('',*,*,#4928,.F.);
#6284=ORIENTED_EDGE('',*,*,#4929,.F.);
#6285=ORIENTED_EDGE('',*,*,#4930,.T.);
#6286=ORIENTED_EDGE('',*,*,#4931,.F.);
#6287=ORIENTED_EDGE('',*,*,#4932,.F.);
#6288=ORIENTED_EDGE('',*,*,#4933,.T.);
#6289=ORIENTED_EDGE('',*,*,#4929,.T.);
#6290=ORIENTED_EDGE('',*,*,#4934,.F.);
#6291=ORIENTED_EDGE('',*,*,#4921,.T.);
#6292=ORIENTED_EDGE('',*,*,#4935,.T.);
#6293=ORIENTED_EDGE('',*,*,#4936,.F.);
#6294=ORIENTED_EDGE('',*,*,#4927,.F.);
#6295=ORIENTED_EDGE('',*,*,#4937,.T.);
#6296=ORIENTED_EDGE('',*,*,#4836,.T.);
#6297=ORIENTED_EDGE('',*,*,#4839,.T.);
#6298=ORIENTED_EDGE('',*,*,#4845,.T.);
#6299=ORIENTED_EDGE('',*,*,#4848,.T.);
#6300=ORIENTED_EDGE('',*,*,#4938,.F.);
#6301=ORIENTED_EDGE('',*,*,#4939,.F.);
#6302=ORIENTED_EDGE('',*,*,#4928,.T.);
#6303=ORIENTED_EDGE('',*,*,#4936,.T.);
#6304=ORIENTED_EDGE('',*,*,#4940,.F.);
#6305=ORIENTED_EDGE('',*,*,#4941,.F.);
#6306=ORIENTED_EDGE('',*,*,#4926,.T.);
#6307=ORIENTED_EDGE('',*,*,#4939,.T.);
#6308=ORIENTED_EDGE('',*,*,#4838,.F.);
#6309=ORIENTED_EDGE('',*,*,#4841,.F.);
#6310=ORIENTED_EDGE('',*,*,#4847,.F.);
#6311=ORIENTED_EDGE('',*,*,#4850,.F.);
#6312=ORIENTED_EDGE('',*,*,#4930,.F.);
#6313=ORIENTED_EDGE('',*,*,#4942,.F.);
#6314=ORIENTED_EDGE('',*,*,#4924,.T.);
#6315=ORIENTED_EDGE('',*,*,#4941,.T.);
#6316=ORIENTED_EDGE('',*,*,#4933,.F.);
#6317=ORIENTED_EDGE('',*,*,#4943,.F.);
#6318=ORIENTED_EDGE('',*,*,#4917,.T.);
#6319=ORIENTED_EDGE('',*,*,#4942,.T.);
#6320=ORIENTED_EDGE('',*,*,#4920,.F.);
#6321=ORIENTED_EDGE('',*,*,#4859,.T.);
#6322=ORIENTED_EDGE('',*,*,#4865,.F.);
#6323=ORIENTED_EDGE('',*,*,#4877,.F.);
#6324=ORIENTED_EDGE('',*,*,#4915,.T.);
#6325=ORIENTED_EDGE('',*,*,#4943,.T.);
#6326=ORIENTED_EDGE('',*,*,#4910,.F.);
#6327=ORIENTED_EDGE('',*,*,#4944,.F.);
#6328=ORIENTED_EDGE('',*,*,#4907,.T.);
#6329=ORIENTED_EDGE('',*,*,#4875,.T.);
#6330=ORIENTED_EDGE('',*,*,#4867,.T.);
#6331=ORIENTED_EDGE('',*,*,#4861,.T.);
#6332=ORIENTED_EDGE('',*,*,#4912,.F.);
#6333=ORIENTED_EDGE('',*,*,#4945,.F.);
#6334=ORIENTED_EDGE('',*,*,#4898,.T.);
#6335=ORIENTED_EDGE('',*,*,#4944,.T.);
#6336=ORIENTED_EDGE('',*,*,#4902,.F.);
#6337=ORIENTED_EDGE('',*,*,#4946,.F.);
#6338=ORIENTED_EDGE('',*,*,#4896,.T.);
#6339=ORIENTED_EDGE('',*,*,#4945,.T.);
#6340=ORIENTED_EDGE('',*,*,#4905,.F.);
#6341=ORIENTED_EDGE('',*,*,#4947,.F.);
#6342=ORIENTED_EDGE('',*,*,#4885,.T.);
#6343=ORIENTED_EDGE('',*,*,#4946,.T.);
#6344=ORIENTED_EDGE('',*,*,#4889,.F.);
#6345=ORIENTED_EDGE('',*,*,#4948,.F.);
#6346=ORIENTED_EDGE('',*,*,#4882,.T.);
#6347=ORIENTED_EDGE('',*,*,#4947,.T.);
#6348=ORIENTED_EDGE('',*,*,#4892,.F.);
#6349=ORIENTED_EDGE('',*,*,#4949,.F.);
#6350=ORIENTED_EDGE('',*,*,#4950,.T.);
#6351=ORIENTED_EDGE('',*,*,#4948,.T.);
#6352=ORIENTED_EDGE('',*,*,#4844,.F.);
#6353=ORIENTED_EDGE('',*,*,#4853,.F.);
#6354=ORIENTED_EDGE('',*,*,#4856,.F.);
#6355=ORIENTED_EDGE('',*,*,#4894,.F.);
#6356=ORIENTED_EDGE('',*,*,#4951,.F.);
#6357=ORIENTED_EDGE('',*,*,#4952,.T.);
#6358=ORIENTED_EDGE('',*,*,#4949,.T.);
#6359=ORIENTED_EDGE('',*,*,#4893,.T.);
#6360=ORIENTED_EDGE('',*,*,#4953,.F.);
#6361=ORIENTED_EDGE('',*,*,#4954,.F.);
#6362=ORIENTED_EDGE('',*,*,#4951,.T.);
#6363=ORIENTED_EDGE('',*,*,#4842,.T.);
#6364=ORIENTED_EDGE('',*,*,#4851,.T.);
#6365=ORIENTED_EDGE('',*,*,#4854,.T.);
#6366=ORIENTED_EDGE('',*,*,#4891,.T.);
#6367=ORIENTED_EDGE('',*,*,#4955,.F.);
#6368=ORIENTED_EDGE('',*,*,#4884,.F.);
#6369=ORIENTED_EDGE('',*,*,#4953,.T.);
#6370=ORIENTED_EDGE('',*,*,#4906,.T.);
#6371=ORIENTED_EDGE('',*,*,#4956,.F.);
#6372=ORIENTED_EDGE('',*,*,#4886,.F.);
#6373=ORIENTED_EDGE('',*,*,#4955,.T.);
#6374=ORIENTED_EDGE('',*,*,#4904,.T.);
#6375=ORIENTED_EDGE('',*,*,#4957,.F.);
#6376=ORIENTED_EDGE('',*,*,#4897,.F.);
#6377=ORIENTED_EDGE('',*,*,#4956,.T.);
#6378=ORIENTED_EDGE('',*,*,#4913,.T.);
#6379=ORIENTED_EDGE('',*,*,#4958,.F.);
#6380=ORIENTED_EDGE('',*,*,#4899,.F.);
#6381=ORIENTED_EDGE('',*,*,#4957,.T.);
#6382=ORIENTED_EDGE('',*,*,#4911,.T.);
#6383=ORIENTED_EDGE('',*,*,#4863,.F.);
#6384=ORIENTED_EDGE('',*,*,#4959,.F.);
#6385=ORIENTED_EDGE('',*,*,#4872,.F.);
#6386=ORIENTED_EDGE('',*,*,#4960,.F.);
#6387=ORIENTED_EDGE('',*,*,#4873,.F.);
#6388=ORIENTED_EDGE('',*,*,#4908,.F.);
#6389=ORIENTED_EDGE('',*,*,#4958,.T.);
#6390=ORIENTED_EDGE('',*,*,#4922,.T.);
#6391=ORIENTED_EDGE('',*,*,#4961,.F.);
#6392=ORIENTED_EDGE('',*,*,#4916,.F.);
#6393=ORIENTED_EDGE('',*,*,#4879,.T.);
#6394=ORIENTED_EDGE('',*,*,#4962,.T.);
#6395=ORIENTED_EDGE('',*,*,#4870,.T.);
#6396=ORIENTED_EDGE('',*,*,#4963,.F.);
#6397=ORIENTED_EDGE('',*,*,#4857,.F.);
#6398=ORIENTED_EDGE('',*,*,#4934,.T.);
#6399=ORIENTED_EDGE('',*,*,#4964,.F.);
#6400=ORIENTED_EDGE('',*,*,#4918,.F.);
#6401=ORIENTED_EDGE('',*,*,#4961,.T.);
#6402=ORIENTED_EDGE('',*,*,#4932,.T.);
#6403=ORIENTED_EDGE('',*,*,#4937,.F.);
#6404=ORIENTED_EDGE('',*,*,#4925,.F.);
#6405=ORIENTED_EDGE('',*,*,#4964,.T.);
#6406=ORIENTED_EDGE('',*,*,#4954,.T.);
#6407=ORIENTED_EDGE('',*,*,#4883,.T.);
#6408=ORIENTED_EDGE('',*,*,#4950,.F.);
#6409=ORIENTED_EDGE('',*,*,#4952,.F.);
#6410=ORIENTED_EDGE('',*,*,#4935,.F.);
#6411=ORIENTED_EDGE('',*,*,#4931,.T.);
#6412=ORIENTED_EDGE('',*,*,#4940,.T.);
#6413=ORIENTED_EDGE('',*,*,#4938,.T.);
#6414=ORIENTED_EDGE('',*,*,#4962,.F.);
#6415=ORIENTED_EDGE('',*,*,#4965,.T.);
#6416=ORIENTED_EDGE('',*,*,#4966,.F.);
#6417=ORIENTED_EDGE('',*,*,#4967,.F.);
#6418=ORIENTED_EDGE('',*,*,#4968,.T.);
#6419=ORIENTED_EDGE('',*,*,#4960,.T.);
#6420=ORIENTED_EDGE('',*,*,#4969,.F.);
#6421=ORIENTED_EDGE('',*,*,#4970,.T.);
#6422=ORIENTED_EDGE('',*,*,#4868,.F.);
#6423=ORIENTED_EDGE('',*,*,#4874,.F.);
#6424=ORIENTED_EDGE('',*,*,#4968,.F.);
#6425=ORIENTED_EDGE('',*,*,#4971,.T.);
#6426=ORIENTED_EDGE('',*,*,#4965,.F.);
#6427=ORIENTED_EDGE('',*,*,#4878,.F.);
#6428=ORIENTED_EDGE('',*,*,#4871,.T.);
#6429=ORIENTED_EDGE('',*,*,#4967,.T.);
#6430=ORIENTED_EDGE('',*,*,#4972,.T.);
#6431=ORIENTED_EDGE('',*,*,#4969,.T.);
#6432=ORIENTED_EDGE('',*,*,#4973,.T.);
#6433=ORIENTED_EDGE('',*,*,#4974,.T.);
#6434=ORIENTED_EDGE('',*,*,#4975,.F.);
#6435=ORIENTED_EDGE('',*,*,#4970,.F.);
#6436=ORIENTED_EDGE('',*,*,#4966,.T.);
#6437=ORIENTED_EDGE('',*,*,#4976,.F.);
#6438=ORIENTED_EDGE('',*,*,#4977,.T.);
#6439=ORIENTED_EDGE('',*,*,#4978,.T.);
#6440=ORIENTED_EDGE('',*,*,#4971,.F.);
#6441=ORIENTED_EDGE('',*,*,#4975,.T.);
#6442=ORIENTED_EDGE('',*,*,#4979,.T.);
#6443=ORIENTED_EDGE('',*,*,#4980,.T.);
#6444=ORIENTED_EDGE('',*,*,#4981,.T.);
#6445=ORIENTED_EDGE('',*,*,#4976,.T.);
#6446=ORIENTED_EDGE('',*,*,#4826,.F.);
#6447=ORIENTED_EDGE('',*,*,#4829,.F.);
#6448=ORIENTED_EDGE('',*,*,#4973,.F.);
#6449=ORIENTED_EDGE('',*,*,#4972,.F.);
#6450=ORIENTED_EDGE('',*,*,#4978,.F.);
#6451=ORIENTED_EDGE('',*,*,#4982,.F.);
#6452=ORIENTED_EDGE('',*,*,#4983,.F.);
#6453=ORIENTED_EDGE('',*,*,#4984,.F.);
#6454=ORIENTED_EDGE('',*,*,#4824,.F.);
#6455=ORIENTED_EDGE('',*,*,#4827,.F.);
#6456=ORIENTED_EDGE('',*,*,#4982,.T.);
#6457=ORIENTED_EDGE('',*,*,#4977,.F.);
#6458=ORIENTED_EDGE('',*,*,#4981,.F.);
#6459=ORIENTED_EDGE('',*,*,#4985,.F.);
#6460=ORIENTED_EDGE('',*,*,#4980,.F.);
#6461=ORIENTED_EDGE('',*,*,#4986,.F.);
#6462=ORIENTED_EDGE('',*,*,#4983,.T.);
#6463=ORIENTED_EDGE('',*,*,#4985,.T.);
#6464=ORIENTED_EDGE('',*,*,#4979,.F.);
#6465=ORIENTED_EDGE('',*,*,#4974,.F.);
#6466=ORIENTED_EDGE('',*,*,#4984,.T.);
#6467=ORIENTED_EDGE('',*,*,#4986,.T.);
#6468=ORIENTED_EDGE('',*,*,#4987,.F.);
#6469=ORIENTED_EDGE('',*,*,#4959,.T.);
#6470=ORIENTED_EDGE('',*,*,#4988,.T.);
#6471=ORIENTED_EDGE('',*,*,#4989,.F.);
#6472=ORIENTED_EDGE('',*,*,#4990,.T.);
#6473=ORIENTED_EDGE('',*,*,#4963,.T.);
#6474=ORIENTED_EDGE('',*,*,#4991,.F.);
#6475=ORIENTED_EDGE('',*,*,#4992,.T.);
#6476=ORIENTED_EDGE('',*,*,#4866,.F.);
#6477=ORIENTED_EDGE('',*,*,#4858,.F.);
#6478=ORIENTED_EDGE('',*,*,#4990,.F.);
#6479=ORIENTED_EDGE('',*,*,#4993,.T.);
#6480=ORIENTED_EDGE('',*,*,#4988,.F.);
#6481=ORIENTED_EDGE('',*,*,#4862,.F.);
#6482=ORIENTED_EDGE('',*,*,#4869,.T.);
#6483=ORIENTED_EDGE('',*,*,#4987,.T.);
#6484=ORIENTED_EDGE('',*,*,#4994,.T.);
#6485=ORIENTED_EDGE('',*,*,#4991,.T.);
#6486=ORIENTED_EDGE('',*,*,#4995,.F.);
#6487=ORIENTED_EDGE('',*,*,#4996,.F.);
#6488=ORIENTED_EDGE('',*,*,#4997,.T.);
#6489=ORIENTED_EDGE('',*,*,#4989,.T.);
#6490=ORIENTED_EDGE('',*,*,#4992,.F.);
#6491=ORIENTED_EDGE('',*,*,#4998,.T.);
#6492=ORIENTED_EDGE('',*,*,#4999,.F.);
#6493=ORIENTED_EDGE('',*,*,#5000,.F.);
#6494=ORIENTED_EDGE('',*,*,#4993,.F.);
#6495=ORIENTED_EDGE('',*,*,#5000,.T.);
#6496=ORIENTED_EDGE('',*,*,#5001,.T.);
#6497=ORIENTED_EDGE('',*,*,#5002,.T.);
#6498=ORIENTED_EDGE('',*,*,#5003,.T.);
#6499=ORIENTED_EDGE('',*,*,#4995,.T.);
#6500=ORIENTED_EDGE('',*,*,#4830,.T.);
#6501=ORIENTED_EDGE('',*,*,#4833,.T.);
#6502=ORIENTED_EDGE('',*,*,#4998,.F.);
#6503=ORIENTED_EDGE('',*,*,#4994,.F.);
#6504=ORIENTED_EDGE('',*,*,#4997,.F.);
#6505=ORIENTED_EDGE('',*,*,#5004,.F.);
#6506=ORIENTED_EDGE('',*,*,#5005,.F.);
#6507=ORIENTED_EDGE('',*,*,#5006,.F.);
#6508=ORIENTED_EDGE('',*,*,#4832,.F.);
#6509=ORIENTED_EDGE('',*,*,#4835,.F.);
#6510=ORIENTED_EDGE('',*,*,#5006,.T.);
#6511=ORIENTED_EDGE('',*,*,#5007,.T.);
#6512=ORIENTED_EDGE('',*,*,#5001,.F.);
#6513=ORIENTED_EDGE('',*,*,#4999,.T.);
#6514=ORIENTED_EDGE('',*,*,#5003,.F.);
#6515=ORIENTED_EDGE('',*,*,#5008,.F.);
#6516=ORIENTED_EDGE('',*,*,#5004,.T.);
#6517=ORIENTED_EDGE('',*,*,#4996,.T.);
#6518=ORIENTED_EDGE('',*,*,#5002,.F.);
#6519=ORIENTED_EDGE('',*,*,#5007,.F.);
#6520=ORIENTED_EDGE('',*,*,#5005,.T.);
#6521=ORIENTED_EDGE('',*,*,#5008,.T.);
#6522=ORIENTED_EDGE('',*,*,#5009,.T.);
#6523=ORIENTED_EDGE('',*,*,#5010,.T.);
#6524=ORIENTED_EDGE('',*,*,#5011,.T.);
#6525=ORIENTED_EDGE('',*,*,#5010,.F.);
#6526=ORIENTED_EDGE('',*,*,#5012,.T.);
#6527=ORIENTED_EDGE('',*,*,#5013,.T.);
#6528=ORIENTED_EDGE('',*,*,#5014,.T.);
#6529=ORIENTED_EDGE('',*,*,#5013,.F.);
#6530=ORIENTED_EDGE('',*,*,#5015,.F.);
#6531=ORIENTED_EDGE('',*,*,#5016,.T.);
#6532=ORIENTED_EDGE('',*,*,#5017,.T.);
#6533=ORIENTED_EDGE('',*,*,#5016,.F.);
#6534=ORIENTED_EDGE('',*,*,#5018,.F.);
#6535=ORIENTED_EDGE('',*,*,#5019,.T.);
#6536=ORIENTED_EDGE('',*,*,#5020,.T.);
#6537=ORIENTED_EDGE('',*,*,#5019,.F.);
#6538=ORIENTED_EDGE('',*,*,#5021,.F.);
#6539=ORIENTED_EDGE('',*,*,#5022,.T.);
#6540=ORIENTED_EDGE('',*,*,#5023,.T.);
#6541=ORIENTED_EDGE('',*,*,#5022,.F.);
#6542=ORIENTED_EDGE('',*,*,#5024,.F.);
#6543=ORIENTED_EDGE('',*,*,#5025,.T.);
#6544=ORIENTED_EDGE('',*,*,#5026,.T.);
#6545=ORIENTED_EDGE('',*,*,#5025,.F.);
#6546=ORIENTED_EDGE('',*,*,#5027,.F.);
#6547=ORIENTED_EDGE('',*,*,#5028,.T.);
#6548=ORIENTED_EDGE('',*,*,#5029,.T.);
#6549=ORIENTED_EDGE('',*,*,#5028,.F.);
#6550=ORIENTED_EDGE('',*,*,#5030,.F.);
#6551=ORIENTED_EDGE('',*,*,#5031,.T.);
#6552=ORIENTED_EDGE('',*,*,#5032,.T.);
#6553=ORIENTED_EDGE('',*,*,#5031,.F.);
#6554=ORIENTED_EDGE('',*,*,#5033,.T.);
#6555=ORIENTED_EDGE('',*,*,#5034,.T.);
#6556=ORIENTED_EDGE('',*,*,#5035,.F.);
#6557=ORIENTED_EDGE('',*,*,#5036,.T.);
#6558=ORIENTED_EDGE('',*,*,#5037,.F.);
#6559=ORIENTED_EDGE('',*,*,#5038,.T.);
#6560=ORIENTED_EDGE('',*,*,#5039,.T.);
#6561=ORIENTED_EDGE('',*,*,#5040,.T.);
#6562=ORIENTED_EDGE('',*,*,#5041,.T.);
#6563=ORIENTED_EDGE('',*,*,#5042,.T.);
#6564=ORIENTED_EDGE('',*,*,#5043,.F.);
#6565=ORIENTED_EDGE('',*,*,#5044,.T.);
#6566=ORIENTED_EDGE('',*,*,#5045,.F.);
#6567=ORIENTED_EDGE('',*,*,#5046,.F.);
#6568=ORIENTED_EDGE('',*,*,#5047,.F.);
#6569=ORIENTED_EDGE('',*,*,#5048,.T.);
#6570=ORIENTED_EDGE('',*,*,#5049,.T.);
#6571=ORIENTED_EDGE('',*,*,#5050,.T.);
#6572=ORIENTED_EDGE('',*,*,#5051,.F.);
#6573=ORIENTED_EDGE('',*,*,#5052,.T.);
#6574=ORIENTED_EDGE('',*,*,#5053,.T.);
#6575=ORIENTED_EDGE('',*,*,#5054,.T.);
#6576=ORIENTED_EDGE('',*,*,#5055,.F.);
#6577=ORIENTED_EDGE('',*,*,#5056,.T.);
#6578=ORIENTED_EDGE('',*,*,#5057,.F.);
#6579=ORIENTED_EDGE('',*,*,#5058,.F.);
#6580=ORIENTED_EDGE('',*,*,#5059,.F.);
#6581=ORIENTED_EDGE('',*,*,#5060,.T.);
#6582=ORIENTED_EDGE('',*,*,#5061,.F.);
#6583=ORIENTED_EDGE('',*,*,#5057,.T.);
#6584=ORIENTED_EDGE('',*,*,#5062,.T.);
#6585=ORIENTED_EDGE('',*,*,#5063,.T.);
#6586=ORIENTED_EDGE('',*,*,#5064,.F.);
#6587=ORIENTED_EDGE('',*,*,#5065,.T.);
#6588=ORIENTED_EDGE('',*,*,#5066,.F.);
#6589=ORIENTED_EDGE('',*,*,#5067,.F.);
#6590=ORIENTED_EDGE('',*,*,#5068,.T.);
#6591=ORIENTED_EDGE('',*,*,#5064,.T.);
#6592=ORIENTED_EDGE('',*,*,#5069,.F.);
#6593=ORIENTED_EDGE('',*,*,#5070,.T.);
#6594=ORIENTED_EDGE('',*,*,#5052,.F.);
#6595=ORIENTED_EDGE('',*,*,#5071,.F.);
#6596=ORIENTED_EDGE('',*,*,#5063,.F.);
#6597=ORIENTED_EDGE('',*,*,#5072,.T.);
#6598=ORIENTED_EDGE('',*,*,#5073,.F.);
#6599=ORIENTED_EDGE('',*,*,#5074,.T.);
#6600=ORIENTED_EDGE('',*,*,#5040,.F.);
#6601=ORIENTED_EDGE('',*,*,#5075,.F.);
#6602=ORIENTED_EDGE('',*,*,#5076,.T.);
#6603=ORIENTED_EDGE('',*,*,#5073,.T.);
#6604=ORIENTED_EDGE('',*,*,#5077,.F.);
#6605=ORIENTED_EDGE('',*,*,#5066,.T.);
#6606=ORIENTED_EDGE('',*,*,#5078,.F.);
#6607=ORIENTED_EDGE('',*,*,#5079,.F.);
#6608=ORIENTED_EDGE('',*,*,#5056,.F.);
#6609=ORIENTED_EDGE('',*,*,#5080,.T.);
#6610=ORIENTED_EDGE('',*,*,#5081,.F.);
#6611=ORIENTED_EDGE('',*,*,#5078,.T.);
#6612=ORIENTED_EDGE('',*,*,#5082,.T.);
#6613=ORIENTED_EDGE('',*,*,#5083,.T.);
#6614=ORIENTED_EDGE('',*,*,#5036,.F.);
#6615=ORIENTED_EDGE('',*,*,#5084,.T.);
#6616=ORIENTED_EDGE('',*,*,#5085,.F.);
#6617=ORIENTED_EDGE('',*,*,#5086,.F.);
#6618=ORIENTED_EDGE('',*,*,#5087,.F.);
#6619=ORIENTED_EDGE('',*,*,#5088,.F.);
#6620=ORIENTED_EDGE('',*,*,#5083,.F.);
#6621=ORIENTED_EDGE('',*,*,#5089,.T.);
#6622=ORIENTED_EDGE('',*,*,#5090,.F.);
#6623=ORIENTED_EDGE('',*,*,#5087,.T.);
#6624=ORIENTED_EDGE('',*,*,#5091,.T.);
#6625=ORIENTED_EDGE('',*,*,#5092,.T.);
#6626=ORIENTED_EDGE('',*,*,#5093,.F.);
#6627=ORIENTED_EDGE('',*,*,#5094,.T.);
#6628=ORIENTED_EDGE('',*,*,#5095,.F.);
#6629=ORIENTED_EDGE('',*,*,#5096,.F.);
#6630=ORIENTED_EDGE('',*,*,#5097,.T.);
#6631=ORIENTED_EDGE('',*,*,#5093,.T.);
#6632=ORIENTED_EDGE('',*,*,#5098,.F.);
#6633=ORIENTED_EDGE('',*,*,#5085,.T.);
#6634=ORIENTED_EDGE('',*,*,#5099,.F.);
#6635=ORIENTED_EDGE('',*,*,#5100,.F.);
#6636=ORIENTED_EDGE('',*,*,#5092,.F.);
#6637=ORIENTED_EDGE('',*,*,#5101,.T.);
#6638=ORIENTED_EDGE('',*,*,#5102,.F.);
#6639=ORIENTED_EDGE('',*,*,#5099,.T.);
#6640=ORIENTED_EDGE('',*,*,#5103,.T.);
#6641=ORIENTED_EDGE('',*,*,#5104,.F.);
#6642=ORIENTED_EDGE('',*,*,#5105,.F.);
#6643=ORIENTED_EDGE('',*,*,#5106,.T.);
#6644=ORIENTED_EDGE('',*,*,#5107,.F.);
#6645=ORIENTED_EDGE('',*,*,#5108,.F.);
#6646=ORIENTED_EDGE('',*,*,#5109,.T.);
#6647=ORIENTED_EDGE('',*,*,#5105,.T.);
#6648=ORIENTED_EDGE('',*,*,#5110,.F.);
#6649=ORIENTED_EDGE('',*,*,#5095,.T.);
#6650=ORIENTED_EDGE('',*,*,#5111,.T.);
#6651=ORIENTED_EDGE('',*,*,#5112,.F.);
#6652=ORIENTED_EDGE('',*,*,#5103,.F.);
#6653=ORIENTED_EDGE('',*,*,#5113,.T.);
#6654=ORIENTED_EDGE('',*,*,#5021,.T.);
#6655=ORIENTED_EDGE('',*,*,#5024,.T.);
#6656=ORIENTED_EDGE('',*,*,#5114,.F.);
#6657=ORIENTED_EDGE('',*,*,#5115,.F.);
#6658=ORIENTED_EDGE('',*,*,#5104,.T.);
#6659=ORIENTED_EDGE('',*,*,#5112,.T.);
#6660=ORIENTED_EDGE('',*,*,#5116,.F.);
#6661=ORIENTED_EDGE('',*,*,#5117,.F.);
#6662=ORIENTED_EDGE('',*,*,#5102,.T.);
#6663=ORIENTED_EDGE('',*,*,#5115,.T.);
#6664=ORIENTED_EDGE('',*,*,#5023,.F.);
#6665=ORIENTED_EDGE('',*,*,#5026,.F.);
#6666=ORIENTED_EDGE('',*,*,#5106,.F.);
#6667=ORIENTED_EDGE('',*,*,#5118,.F.);
#6668=ORIENTED_EDGE('',*,*,#5100,.T.);
#6669=ORIENTED_EDGE('',*,*,#5117,.T.);
#6670=ORIENTED_EDGE('',*,*,#5109,.F.);
#6671=ORIENTED_EDGE('',*,*,#5119,.F.);
#6672=ORIENTED_EDGE('',*,*,#5090,.T.);
#6673=ORIENTED_EDGE('',*,*,#5118,.T.);
#6674=ORIENTED_EDGE('',*,*,#5094,.F.);
#6675=ORIENTED_EDGE('',*,*,#5120,.F.);
#6676=ORIENTED_EDGE('',*,*,#5088,.T.);
#6677=ORIENTED_EDGE('',*,*,#5119,.T.);
#6678=ORIENTED_EDGE('',*,*,#5097,.F.);
#6679=ORIENTED_EDGE('',*,*,#5121,.F.);
#6680=ORIENTED_EDGE('',*,*,#5081,.T.);
#6681=ORIENTED_EDGE('',*,*,#5120,.T.);
#6682=ORIENTED_EDGE('',*,*,#5084,.F.);
#6683=ORIENTED_EDGE('',*,*,#5035,.T.);
#6684=ORIENTED_EDGE('',*,*,#5041,.F.);
#6685=ORIENTED_EDGE('',*,*,#5053,.F.);
#6686=ORIENTED_EDGE('',*,*,#5079,.T.);
#6687=ORIENTED_EDGE('',*,*,#5121,.T.);
#6688=ORIENTED_EDGE('',*,*,#5074,.F.);
#6689=ORIENTED_EDGE('',*,*,#5122,.F.);
#6690=ORIENTED_EDGE('',*,*,#5071,.T.);
#6691=ORIENTED_EDGE('',*,*,#5051,.T.);
#6692=ORIENTED_EDGE('',*,*,#5043,.T.);
#6693=ORIENTED_EDGE('',*,*,#5037,.T.);
#6694=ORIENTED_EDGE('',*,*,#5076,.F.);
#6695=ORIENTED_EDGE('',*,*,#5123,.F.);
#6696=ORIENTED_EDGE('',*,*,#5061,.T.);
#6697=ORIENTED_EDGE('',*,*,#5122,.T.);
#6698=ORIENTED_EDGE('',*,*,#5065,.F.);
#6699=ORIENTED_EDGE('',*,*,#5124,.F.);
#6700=ORIENTED_EDGE('',*,*,#5058,.T.);
#6701=ORIENTED_EDGE('',*,*,#5123,.T.);
#6702=ORIENTED_EDGE('',*,*,#5068,.F.);
#6703=ORIENTED_EDGE('',*,*,#5125,.F.);
#6704=ORIENTED_EDGE('',*,*,#5126,.T.);
#6705=ORIENTED_EDGE('',*,*,#5124,.T.);
#6706=ORIENTED_EDGE('',*,*,#5029,.F.);
#6707=ORIENTED_EDGE('',*,*,#5032,.F.);
#6708=ORIENTED_EDGE('',*,*,#5070,.F.);
#6709=ORIENTED_EDGE('',*,*,#5127,.F.);
#6710=ORIENTED_EDGE('',*,*,#5128,.T.);
#6711=ORIENTED_EDGE('',*,*,#5125,.T.);
#6712=ORIENTED_EDGE('',*,*,#5069,.T.);
#6713=ORIENTED_EDGE('',*,*,#5129,.F.);
#6714=ORIENTED_EDGE('',*,*,#5130,.F.);
#6715=ORIENTED_EDGE('',*,*,#5127,.T.);
#6716=ORIENTED_EDGE('',*,*,#5027,.T.);
#6717=ORIENTED_EDGE('',*,*,#5030,.T.);
#6718=ORIENTED_EDGE('',*,*,#5067,.T.);
#6719=ORIENTED_EDGE('',*,*,#5131,.F.);
#6720=ORIENTED_EDGE('',*,*,#5060,.F.);
#6721=ORIENTED_EDGE('',*,*,#5129,.T.);
#6722=ORIENTED_EDGE('',*,*,#5077,.T.);
#6723=ORIENTED_EDGE('',*,*,#5132,.F.);
#6724=ORIENTED_EDGE('',*,*,#5062,.F.);
#6725=ORIENTED_EDGE('',*,*,#5131,.T.);
#6726=ORIENTED_EDGE('',*,*,#5075,.T.);
#6727=ORIENTED_EDGE('',*,*,#5039,.F.);
#6728=ORIENTED_EDGE('',*,*,#5133,.F.);
#6729=ORIENTED_EDGE('',*,*,#5048,.F.);
#6730=ORIENTED_EDGE('',*,*,#5134,.F.);
#6731=ORIENTED_EDGE('',*,*,#5049,.F.);
#6732=ORIENTED_EDGE('',*,*,#5072,.F.);
#6733=ORIENTED_EDGE('',*,*,#5132,.T.);
#6734=ORIENTED_EDGE('',*,*,#5086,.T.);
#6735=ORIENTED_EDGE('',*,*,#5135,.F.);
#6736=ORIENTED_EDGE('',*,*,#5080,.F.);
#6737=ORIENTED_EDGE('',*,*,#5055,.T.);
#6738=ORIENTED_EDGE('',*,*,#5136,.T.);
#6739=ORIENTED_EDGE('',*,*,#5046,.T.);
#6740=ORIENTED_EDGE('',*,*,#5137,.F.);
#6741=ORIENTED_EDGE('',*,*,#5033,.F.);
#6742=ORIENTED_EDGE('',*,*,#5098,.T.);
#6743=ORIENTED_EDGE('',*,*,#5138,.F.);
#6744=ORIENTED_EDGE('',*,*,#5082,.F.);
#6745=ORIENTED_EDGE('',*,*,#5135,.T.);
#6746=ORIENTED_EDGE('',*,*,#5096,.T.);
#6747=ORIENTED_EDGE('',*,*,#5139,.F.);
#6748=ORIENTED_EDGE('',*,*,#5089,.F.);
#6749=ORIENTED_EDGE('',*,*,#5138,.T.);
#6750=ORIENTED_EDGE('',*,*,#5110,.T.);
#6751=ORIENTED_EDGE('',*,*,#5140,.F.);
#6752=ORIENTED_EDGE('',*,*,#5091,.F.);
#6753=ORIENTED_EDGE('',*,*,#5139,.T.);
#6754=ORIENTED_EDGE('',*,*,#5108,.T.);
#6755=ORIENTED_EDGE('',*,*,#5113,.F.);
#6756=ORIENTED_EDGE('',*,*,#5101,.F.);
#6757=ORIENTED_EDGE('',*,*,#5140,.T.);
#6758=ORIENTED_EDGE('',*,*,#5130,.T.);
#6759=ORIENTED_EDGE('',*,*,#5059,.T.);
#6760=ORIENTED_EDGE('',*,*,#5126,.F.);
#6761=ORIENTED_EDGE('',*,*,#5128,.F.);
#6762=ORIENTED_EDGE('',*,*,#5111,.F.);
#6763=ORIENTED_EDGE('',*,*,#5107,.T.);
#6764=ORIENTED_EDGE('',*,*,#5116,.T.);
#6765=ORIENTED_EDGE('',*,*,#5114,.T.);
#6766=ORIENTED_EDGE('',*,*,#5136,.F.);
#6767=ORIENTED_EDGE('',*,*,#5141,.T.);
#6768=ORIENTED_EDGE('',*,*,#5142,.F.);
#6769=ORIENTED_EDGE('',*,*,#5143,.F.);
#6770=ORIENTED_EDGE('',*,*,#5144,.T.);
#6771=ORIENTED_EDGE('',*,*,#5134,.T.);
#6772=ORIENTED_EDGE('',*,*,#5145,.F.);
#6773=ORIENTED_EDGE('',*,*,#5146,.T.);
#6774=ORIENTED_EDGE('',*,*,#5044,.F.);
#6775=ORIENTED_EDGE('',*,*,#5050,.F.);
#6776=ORIENTED_EDGE('',*,*,#5144,.F.);
#6777=ORIENTED_EDGE('',*,*,#5147,.T.);
#6778=ORIENTED_EDGE('',*,*,#5141,.F.);
#6779=ORIENTED_EDGE('',*,*,#5054,.F.);
#6780=ORIENTED_EDGE('',*,*,#5047,.T.);
#6781=ORIENTED_EDGE('',*,*,#5143,.T.);
#6782=ORIENTED_EDGE('',*,*,#5148,.T.);
#6783=ORIENTED_EDGE('',*,*,#5145,.T.);
#6784=ORIENTED_EDGE('',*,*,#5146,.F.);
#6785=ORIENTED_EDGE('',*,*,#5149,.T.);
#6786=ORIENTED_EDGE('',*,*,#5150,.F.);
#6787=ORIENTED_EDGE('',*,*,#5151,.F.);
#6788=ORIENTED_EDGE('',*,*,#5152,.F.);
#6789=ORIENTED_EDGE('',*,*,#5153,.F.);
#6790=ORIENTED_EDGE('',*,*,#5154,.T.);
#6791=ORIENTED_EDGE('',*,*,#5142,.T.);
#6792=ORIENTED_EDGE('',*,*,#5147,.F.);
#6793=ORIENTED_EDGE('',*,*,#5151,.T.);
#6794=ORIENTED_EDGE('',*,*,#5155,.T.);
#6795=ORIENTED_EDGE('',*,*,#5156,.T.);
#6796=ORIENTED_EDGE('',*,*,#5157,.T.);
#6797=ORIENTED_EDGE('',*,*,#5152,.T.);
#6798=ORIENTED_EDGE('',*,*,#5011,.F.);
#6799=ORIENTED_EDGE('',*,*,#5014,.F.);
#6800=ORIENTED_EDGE('',*,*,#5149,.F.);
#6801=ORIENTED_EDGE('',*,*,#5148,.F.);
#6802=ORIENTED_EDGE('',*,*,#5154,.F.);
#6803=ORIENTED_EDGE('',*,*,#5158,.F.);
#6804=ORIENTED_EDGE('',*,*,#5159,.F.);
#6805=ORIENTED_EDGE('',*,*,#5160,.F.);
#6806=ORIENTED_EDGE('',*,*,#5009,.F.);
#6807=ORIENTED_EDGE('',*,*,#5012,.F.);
#6808=ORIENTED_EDGE('',*,*,#5160,.T.);
#6809=ORIENTED_EDGE('',*,*,#5161,.T.);
#6810=ORIENTED_EDGE('',*,*,#5155,.F.);
#6811=ORIENTED_EDGE('',*,*,#5150,.T.);
#6812=ORIENTED_EDGE('',*,*,#5157,.F.);
#6813=ORIENTED_EDGE('',*,*,#5162,.F.);
#6814=ORIENTED_EDGE('',*,*,#5158,.T.);
#6815=ORIENTED_EDGE('',*,*,#5153,.T.);
#6816=ORIENTED_EDGE('',*,*,#5156,.F.);
#6817=ORIENTED_EDGE('',*,*,#5161,.F.);
#6818=ORIENTED_EDGE('',*,*,#5159,.T.);
#6819=ORIENTED_EDGE('',*,*,#5162,.T.);
#6820=ORIENTED_EDGE('',*,*,#5163,.F.);
#6821=ORIENTED_EDGE('',*,*,#5133,.T.);
#6822=ORIENTED_EDGE('',*,*,#5164,.T.);
#6823=ORIENTED_EDGE('',*,*,#5165,.F.);
#6824=ORIENTED_EDGE('',*,*,#5166,.T.);
#6825=ORIENTED_EDGE('',*,*,#5137,.T.);
#6826=ORIENTED_EDGE('',*,*,#5167,.F.);
#6827=ORIENTED_EDGE('',*,*,#5168,.T.);
#6828=ORIENTED_EDGE('',*,*,#5042,.F.);
#6829=ORIENTED_EDGE('',*,*,#5034,.F.);
#6830=ORIENTED_EDGE('',*,*,#5166,.F.);
#6831=ORIENTED_EDGE('',*,*,#5169,.T.);
#6832=ORIENTED_EDGE('',*,*,#5164,.F.);
#6833=ORIENTED_EDGE('',*,*,#5038,.F.);
#6834=ORIENTED_EDGE('',*,*,#5045,.T.);
#6835=ORIENTED_EDGE('',*,*,#5163,.T.);
#6836=ORIENTED_EDGE('',*,*,#5170,.T.);
#6837=ORIENTED_EDGE('',*,*,#5167,.T.);
#6838=ORIENTED_EDGE('',*,*,#5165,.T.);
#6839=ORIENTED_EDGE('',*,*,#5171,.F.);
#6840=ORIENTED_EDGE('',*,*,#5172,.T.);
#6841=ORIENTED_EDGE('',*,*,#5173,.T.);
#6842=ORIENTED_EDGE('',*,*,#5174,.T.);
#6843=ORIENTED_EDGE('',*,*,#5175,.T.);
#6844=ORIENTED_EDGE('',*,*,#5176,.F.);
#6845=ORIENTED_EDGE('',*,*,#5168,.F.);
#6846=ORIENTED_EDGE('',*,*,#5169,.F.);
#6847=ORIENTED_EDGE('',*,*,#5176,.T.);
#6848=ORIENTED_EDGE('',*,*,#5177,.T.);
#6849=ORIENTED_EDGE('',*,*,#5178,.T.);
#6850=ORIENTED_EDGE('',*,*,#5179,.T.);
#6851=ORIENTED_EDGE('',*,*,#5171,.T.);
#6852=ORIENTED_EDGE('',*,*,#5015,.T.);
#6853=ORIENTED_EDGE('',*,*,#5018,.T.);
#6854=ORIENTED_EDGE('',*,*,#5174,.F.);
#6855=ORIENTED_EDGE('',*,*,#5170,.F.);
#6856=ORIENTED_EDGE('',*,*,#5173,.F.);
#6857=ORIENTED_EDGE('',*,*,#5180,.F.);
#6858=ORIENTED_EDGE('',*,*,#5181,.F.);
#6859=ORIENTED_EDGE('',*,*,#5182,.F.);
#6860=ORIENTED_EDGE('',*,*,#5017,.F.);
#6861=ORIENTED_EDGE('',*,*,#5020,.F.);
#6862=ORIENTED_EDGE('',*,*,#5180,.T.);
#6863=ORIENTED_EDGE('',*,*,#5172,.F.);
#6864=ORIENTED_EDGE('',*,*,#5179,.F.);
#6865=ORIENTED_EDGE('',*,*,#5183,.F.);
#6866=ORIENTED_EDGE('',*,*,#5178,.F.);
#6867=ORIENTED_EDGE('',*,*,#5184,.F.);
#6868=ORIENTED_EDGE('',*,*,#5181,.T.);
#6869=ORIENTED_EDGE('',*,*,#5183,.T.);
#6870=ORIENTED_EDGE('',*,*,#5177,.F.);
#6871=ORIENTED_EDGE('',*,*,#5175,.F.);
#6872=ORIENTED_EDGE('',*,*,#5182,.T.);
#6873=ORIENTED_EDGE('',*,*,#5184,.T.);
#6874=ORIENTED_EDGE('',*,*,#5185,.F.);
#6875=ORIENTED_EDGE('',*,*,#5186,.T.);
#6876=ORIENTED_EDGE('',*,*,#5187,.T.);
#6877=ORIENTED_EDGE('',*,*,#5186,.F.);
#6878=ORIENTED_EDGE('',*,*,#5188,.F.);
#6879=ORIENTED_EDGE('',*,*,#5189,.T.);
#6880=ORIENTED_EDGE('',*,*,#5190,.T.);
#6881=ORIENTED_EDGE('',*,*,#5189,.F.);
#6882=ORIENTED_EDGE('',*,*,#5191,.F.);
#6883=ORIENTED_EDGE('',*,*,#5192,.T.);
#6884=ORIENTED_EDGE('',*,*,#5193,.T.);
#6885=ORIENTED_EDGE('',*,*,#5192,.F.);
#6886=ORIENTED_EDGE('',*,*,#5194,.F.);
#6887=ORIENTED_EDGE('',*,*,#5195,.T.);
#6888=ORIENTED_EDGE('',*,*,#5196,.T.);
#6889=ORIENTED_EDGE('',*,*,#5195,.F.);
#6890=ORIENTED_EDGE('',*,*,#5197,.F.);
#6891=ORIENTED_EDGE('',*,*,#5198,.T.);
#6892=ORIENTED_EDGE('',*,*,#5199,.T.);
#6893=ORIENTED_EDGE('',*,*,#5198,.F.);
#6894=ORIENTED_EDGE('',*,*,#5200,.F.);
#6895=ORIENTED_EDGE('',*,*,#5201,.T.);
#6896=ORIENTED_EDGE('',*,*,#5202,.T.);
#6897=ORIENTED_EDGE('',*,*,#5201,.F.);
#6898=ORIENTED_EDGE('',*,*,#5203,.F.);
#6899=ORIENTED_EDGE('',*,*,#5204,.T.);
#6900=ORIENTED_EDGE('',*,*,#5205,.T.);
#6901=ORIENTED_EDGE('',*,*,#5204,.F.);
#6902=ORIENTED_EDGE('',*,*,#5206,.F.);
#6903=ORIENTED_EDGE('',*,*,#5207,.T.);
#6904=ORIENTED_EDGE('',*,*,#5208,.T.);
#6905=ORIENTED_EDGE('',*,*,#5207,.F.);
#6906=ORIENTED_EDGE('',*,*,#5209,.T.);
#6907=ORIENTED_EDGE('',*,*,#5210,.T.);
#6908=ORIENTED_EDGE('',*,*,#5211,.F.);
#6909=ORIENTED_EDGE('',*,*,#5212,.T.);
#6910=ORIENTED_EDGE('',*,*,#5213,.F.);
#6911=ORIENTED_EDGE('',*,*,#5214,.T.);
#6912=ORIENTED_EDGE('',*,*,#5215,.F.);
#6913=ORIENTED_EDGE('',*,*,#5216,.F.);
#6914=ORIENTED_EDGE('',*,*,#5217,.T.);
#6915=ORIENTED_EDGE('',*,*,#5213,.T.);
#6916=ORIENTED_EDGE('',*,*,#5218,.F.);
#6917=ORIENTED_EDGE('',*,*,#5219,.F.);
#6918=ORIENTED_EDGE('',*,*,#5220,.F.);
#6919=ORIENTED_EDGE('',*,*,#5221,.F.);
#6920=ORIENTED_EDGE('',*,*,#5222,.F.);
#6921=ORIENTED_EDGE('',*,*,#5223,.T.);
#6922=ORIENTED_EDGE('',*,*,#5224,.F.);
#6923=ORIENTED_EDGE('',*,*,#5220,.T.);
#6924=ORIENTED_EDGE('',*,*,#5225,.T.);
#6925=ORIENTED_EDGE('',*,*,#5226,.T.);
#6926=ORIENTED_EDGE('',*,*,#5227,.F.);
#6927=ORIENTED_EDGE('',*,*,#5228,.T.);
#6928=ORIENTED_EDGE('',*,*,#5229,.F.);
#6929=ORIENTED_EDGE('',*,*,#5230,.F.);
#6930=ORIENTED_EDGE('',*,*,#5231,.T.);
#6931=ORIENTED_EDGE('',*,*,#5227,.T.);
#6932=ORIENTED_EDGE('',*,*,#5232,.F.);
#6933=ORIENTED_EDGE('',*,*,#5215,.T.);
#6934=ORIENTED_EDGE('',*,*,#5212,.F.);
#6935=ORIENTED_EDGE('',*,*,#5233,.F.);
#6936=ORIENTED_EDGE('',*,*,#5226,.F.);
#6937=ORIENTED_EDGE('',*,*,#5234,.T.);
#6938=ORIENTED_EDGE('',*,*,#5235,.F.);
#6939=ORIENTED_EDGE('',*,*,#5236,.F.);
#6940=ORIENTED_EDGE('',*,*,#5229,.T.);
#6941=ORIENTED_EDGE('',*,*,#5237,.T.);
#6942=ORIENTED_EDGE('',*,*,#5238,.T.);
#6943=ORIENTED_EDGE('',*,*,#5239,.T.);
#6944=ORIENTED_EDGE('',*,*,#5240,.F.);
#6945=ORIENTED_EDGE('',*,*,#5241,.T.);
#6946=ORIENTED_EDGE('',*,*,#5242,.T.);
#6947=ORIENTED_EDGE('',*,*,#5243,.F.);
#6948=ORIENTED_EDGE('',*,*,#5244,.F.);
#6949=ORIENTED_EDGE('',*,*,#5240,.T.);
#6950=ORIENTED_EDGE('',*,*,#5245,.F.);
#6951=ORIENTED_EDGE('',*,*,#5246,.F.);
#6952=ORIENTED_EDGE('',*,*,#5247,.F.);
#6953=ORIENTED_EDGE('',*,*,#5243,.T.);
#6954=ORIENTED_EDGE('',*,*,#5248,.F.);
#6955=ORIENTED_EDGE('',*,*,#5249,.F.);
#6956=ORIENTED_EDGE('',*,*,#5250,.F.);
#6957=ORIENTED_EDGE('',*,*,#5246,.T.);
#6958=ORIENTED_EDGE('',*,*,#5251,.F.);
#6959=ORIENTED_EDGE('',*,*,#5252,.T.);
#6960=ORIENTED_EDGE('',*,*,#5209,.F.);
#6961=ORIENTED_EDGE('',*,*,#5253,.F.);
#6962=ORIENTED_EDGE('',*,*,#5236,.T.);
#6963=ORIENTED_EDGE('',*,*,#5254,.F.);
#6964=ORIENTED_EDGE('',*,*,#5255,.F.);
#6965=ORIENTED_EDGE('',*,*,#5249,.T.);
#6966=ORIENTED_EDGE('',*,*,#5234,.F.);
#6967=ORIENTED_EDGE('',*,*,#5256,.F.);
#6968=ORIENTED_EDGE('',*,*,#5230,.T.);
#6969=ORIENTED_EDGE('',*,*,#5253,.T.);
#6970=ORIENTED_EDGE('',*,*,#5225,.F.);
#6971=ORIENTED_EDGE('',*,*,#5257,.F.);
#6972=ORIENTED_EDGE('',*,*,#5232,.T.);
#6973=ORIENTED_EDGE('',*,*,#5256,.T.);
#6974=ORIENTED_EDGE('',*,*,#5187,.F.);
#6975=ORIENTED_EDGE('',*,*,#5190,.F.);
#6976=ORIENTED_EDGE('',*,*,#5193,.F.);
#6977=ORIENTED_EDGE('',*,*,#5196,.F.);
#6978=ORIENTED_EDGE('',*,*,#5223,.F.);
#6979=ORIENTED_EDGE('',*,*,#5258,.F.);
#6980=ORIENTED_EDGE('',*,*,#5216,.T.);
#6981=ORIENTED_EDGE('',*,*,#5257,.T.);
#6982=ORIENTED_EDGE('',*,*,#5259,.F.);
#6983=ORIENTED_EDGE('',*,*,#5260,.F.);
#6984=ORIENTED_EDGE('',*,*,#5218,.T.);
#6985=ORIENTED_EDGE('',*,*,#5258,.T.);
#6986=ORIENTED_EDGE('',*,*,#5199,.F.);
#6987=ORIENTED_EDGE('',*,*,#5202,.F.);
#6988=ORIENTED_EDGE('',*,*,#5205,.F.);
#6989=ORIENTED_EDGE('',*,*,#5208,.F.);
#6990=ORIENTED_EDGE('',*,*,#5261,.F.);
#6991=ORIENTED_EDGE('',*,*,#5262,.F.);
#6992=ORIENTED_EDGE('',*,*,#5219,.T.);
#6993=ORIENTED_EDGE('',*,*,#5260,.T.);
#6994=ORIENTED_EDGE('',*,*,#5263,.T.);
#6995=ORIENTED_EDGE('',*,*,#5264,.F.);
#6996=ORIENTED_EDGE('',*,*,#5217,.F.);
#6997=ORIENTED_EDGE('',*,*,#5262,.T.);
#6998=ORIENTED_EDGE('',*,*,#5197,.T.);
#6999=ORIENTED_EDGE('',*,*,#5200,.T.);
#7000=ORIENTED_EDGE('',*,*,#5203,.T.);
#7001=ORIENTED_EDGE('',*,*,#5206,.T.);
#7002=ORIENTED_EDGE('',*,*,#5221,.T.);
#7003=ORIENTED_EDGE('',*,*,#5265,.F.);
#7004=ORIENTED_EDGE('',*,*,#5214,.F.);
#7005=ORIENTED_EDGE('',*,*,#5264,.T.);
#7006=ORIENTED_EDGE('',*,*,#5224,.T.);
#7007=ORIENTED_EDGE('',*,*,#5266,.F.);
#7008=ORIENTED_EDGE('',*,*,#5231,.F.);
#7009=ORIENTED_EDGE('',*,*,#5265,.T.);
#7010=ORIENTED_EDGE('',*,*,#5185,.T.);
#7011=ORIENTED_EDGE('',*,*,#5188,.T.);
#7012=ORIENTED_EDGE('',*,*,#5191,.T.);
#7013=ORIENTED_EDGE('',*,*,#5194,.T.);
#7014=ORIENTED_EDGE('',*,*,#5233,.T.);
#7015=ORIENTED_EDGE('',*,*,#5267,.F.);
#7016=ORIENTED_EDGE('',*,*,#5228,.F.);
#7017=ORIENTED_EDGE('',*,*,#5266,.T.);
#7018=ORIENTED_EDGE('',*,*,#5268,.F.);
#7019=ORIENTED_EDGE('',*,*,#5269,.T.);
#7020=ORIENTED_EDGE('',*,*,#5270,.F.);
#7021=ORIENTED_EDGE('',*,*,#5271,.T.);
#7022=ORIENTED_EDGE('',*,*,#5272,.T.);
#7023=ORIENTED_EDGE('',*,*,#5237,.F.);
#7024=ORIENTED_EDGE('',*,*,#5267,.T.);
#7025=ORIENTED_EDGE('',*,*,#5211,.T.);
#7026=ORIENTED_EDGE('',*,*,#5270,.T.);
#7027=ORIENTED_EDGE('',*,*,#5273,.T.);
#7028=ORIENTED_EDGE('',*,*,#5238,.F.);
#7029=ORIENTED_EDGE('',*,*,#5274,.T.);
#7030=ORIENTED_EDGE('',*,*,#5259,.T.);
#7031=ORIENTED_EDGE('',*,*,#5222,.T.);
#7032=ORIENTED_EDGE('',*,*,#5263,.F.);
#7033=ORIENTED_EDGE('',*,*,#5261,.T.);
#7034=ORIENTED_EDGE('',*,*,#5254,.T.);
#7035=ORIENTED_EDGE('',*,*,#5235,.T.);
#7036=ORIENTED_EDGE('',*,*,#5272,.F.);
#7037=ORIENTED_EDGE('',*,*,#5275,.T.);
#7038=ORIENTED_EDGE('',*,*,#5250,.T.);
#7039=ORIENTED_EDGE('',*,*,#5255,.T.);
#7040=ORIENTED_EDGE('',*,*,#5275,.F.);
#7041=ORIENTED_EDGE('',*,*,#5271,.F.);
#7042=ORIENTED_EDGE('',*,*,#5274,.F.);
#7043=ORIENTED_EDGE('',*,*,#5241,.F.);
#7044=ORIENTED_EDGE('',*,*,#5244,.T.);
#7045=ORIENTED_EDGE('',*,*,#5247,.T.);
#7046=ORIENTED_EDGE('',*,*,#5248,.T.);
#7047=ORIENTED_EDGE('',*,*,#5245,.T.);
#7048=ORIENTED_EDGE('',*,*,#5242,.F.);
#7049=ORIENTED_EDGE('',*,*,#5239,.F.);
#7050=ORIENTED_EDGE('',*,*,#5273,.F.);
#7051=ORIENTED_EDGE('',*,*,#5269,.F.);
#7052=ORIENTED_EDGE('',*,*,#5276,.F.);
#7053=ORIENTED_EDGE('',*,*,#5251,.T.);
#7054=ORIENTED_EDGE('',*,*,#5276,.T.);
#7055=ORIENTED_EDGE('',*,*,#5268,.T.);
#7056=ORIENTED_EDGE('',*,*,#5210,.F.);
#7057=ORIENTED_EDGE('',*,*,#5252,.F.);
#7058=ORIENTED_EDGE('',*,*,#5277,.F.);
#7059=ORIENTED_EDGE('',*,*,#5278,.T.);
#7060=ORIENTED_EDGE('',*,*,#5279,.T.);
#7061=ORIENTED_EDGE('',*,*,#5278,.F.);
#7062=ORIENTED_EDGE('',*,*,#5280,.T.);
#7063=ORIENTED_EDGE('',*,*,#5281,.T.);
#7064=ORIENTED_EDGE('',*,*,#5282,.F.);
#7065=ORIENTED_EDGE('',*,*,#5281,.F.);
#7066=ORIENTED_EDGE('',*,*,#5283,.T.);
#7067=ORIENTED_EDGE('',*,*,#5284,.T.);
#7068=ORIENTED_EDGE('',*,*,#5285,.F.);
#7069=ORIENTED_EDGE('',*,*,#5284,.F.);
#7070=ORIENTED_EDGE('',*,*,#5286,.T.);
#7071=ORIENTED_EDGE('',*,*,#5287,.T.);
#7072=ORIENTED_EDGE('',*,*,#5288,.F.);
#7073=ORIENTED_EDGE('',*,*,#5287,.F.);
#7074=ORIENTED_EDGE('',*,*,#5289,.T.);
#7075=ORIENTED_EDGE('',*,*,#5290,.T.);
#7076=ORIENTED_EDGE('',*,*,#5291,.F.);
#7077=ORIENTED_EDGE('',*,*,#5290,.F.);
#7078=ORIENTED_EDGE('',*,*,#5292,.T.);
#7079=ORIENTED_EDGE('',*,*,#5293,.T.);
#7080=ORIENTED_EDGE('',*,*,#5294,.F.);
#7081=ORIENTED_EDGE('',*,*,#5293,.F.);
#7082=ORIENTED_EDGE('',*,*,#5295,.T.);
#7083=ORIENTED_EDGE('',*,*,#5296,.T.);
#7084=ORIENTED_EDGE('',*,*,#5297,.F.);
#7085=ORIENTED_EDGE('',*,*,#5296,.F.);
#7086=ORIENTED_EDGE('',*,*,#5298,.T.);
#7087=ORIENTED_EDGE('',*,*,#5299,.T.);
#7088=ORIENTED_EDGE('',*,*,#5300,.F.);
#7089=ORIENTED_EDGE('',*,*,#5299,.F.);
#7090=ORIENTED_EDGE('',*,*,#5301,.F.);
#7091=ORIENTED_EDGE('',*,*,#5302,.F.);
#7092=ORIENTED_EDGE('',*,*,#5303,.T.);
#7093=ORIENTED_EDGE('',*,*,#5304,.F.);
#7094=ORIENTED_EDGE('',*,*,#5305,.T.);
#7095=ORIENTED_EDGE('',*,*,#5306,.T.);
#7096=ORIENTED_EDGE('',*,*,#5307,.T.);
#7097=ORIENTED_EDGE('',*,*,#5308,.F.);
#7098=ORIENTED_EDGE('',*,*,#5309,.F.);
#7099=ORIENTED_EDGE('',*,*,#5310,.T.);
#7100=ORIENTED_EDGE('',*,*,#5311,.T.);
#7101=ORIENTED_EDGE('',*,*,#5305,.F.);
#7102=ORIENTED_EDGE('',*,*,#5312,.T.);
#7103=ORIENTED_EDGE('',*,*,#5313,.F.);
#7104=ORIENTED_EDGE('',*,*,#5314,.T.);
#7105=ORIENTED_EDGE('',*,*,#5315,.T.);
#7106=ORIENTED_EDGE('',*,*,#5316,.T.);
#7107=ORIENTED_EDGE('',*,*,#5317,.F.);
#7108=ORIENTED_EDGE('',*,*,#5318,.F.);
#7109=ORIENTED_EDGE('',*,*,#5312,.F.);
#7110=ORIENTED_EDGE('',*,*,#5319,.T.);
#7111=ORIENTED_EDGE('',*,*,#5320,.T.);
#7112=ORIENTED_EDGE('',*,*,#5321,.T.);
#7113=ORIENTED_EDGE('',*,*,#5322,.F.);
#7114=ORIENTED_EDGE('',*,*,#5323,.F.);
#7115=ORIENTED_EDGE('',*,*,#5307,.F.);
#7116=ORIENTED_EDGE('',*,*,#5324,.T.);
#7117=ORIENTED_EDGE('',*,*,#5319,.F.);
#7118=ORIENTED_EDGE('',*,*,#5302,.T.);
#7119=ORIENTED_EDGE('',*,*,#5325,.F.);
#7120=ORIENTED_EDGE('',*,*,#5317,.T.);
#7121=ORIENTED_EDGE('',*,*,#5326,.T.);
#7122=ORIENTED_EDGE('',*,*,#5327,.T.);
#7123=ORIENTED_EDGE('',*,*,#5328,.F.);
#7124=ORIENTED_EDGE('',*,*,#5321,.F.);
#7125=ORIENTED_EDGE('',*,*,#5329,.T.);
#7126=ORIENTED_EDGE('',*,*,#5330,.F.);
#7127=ORIENTED_EDGE('',*,*,#5331,.F.);
#7128=ORIENTED_EDGE('',*,*,#5332,.T.);
#7129=ORIENTED_EDGE('',*,*,#5333,.F.);
#7130=ORIENTED_EDGE('',*,*,#5334,.F.);
#7131=ORIENTED_EDGE('',*,*,#5332,.F.);
#7132=ORIENTED_EDGE('',*,*,#5335,.T.);
#7133=ORIENTED_EDGE('',*,*,#5336,.T.);
#7134=ORIENTED_EDGE('',*,*,#5337,.T.);
#7135=ORIENTED_EDGE('',*,*,#5336,.F.);
#7136=ORIENTED_EDGE('',*,*,#5338,.T.);
#7137=ORIENTED_EDGE('',*,*,#5339,.T.);
#7138=ORIENTED_EDGE('',*,*,#5340,.T.);
#7139=ORIENTED_EDGE('',*,*,#5339,.F.);
#7140=ORIENTED_EDGE('',*,*,#5341,.T.);
#7141=ORIENTED_EDGE('',*,*,#5342,.T.);
#7142=ORIENTED_EDGE('',*,*,#5343,.T.);
#7143=ORIENTED_EDGE('',*,*,#5342,.F.);
#7144=ORIENTED_EDGE('',*,*,#5344,.T.);
#7145=ORIENTED_EDGE('',*,*,#5345,.T.);
#7146=ORIENTED_EDGE('',*,*,#5329,.F.);
#7147=ORIENTED_EDGE('',*,*,#5346,.T.);
#7148=ORIENTED_EDGE('',*,*,#5301,.T.);
#7149=ORIENTED_EDGE('',*,*,#5347,.F.);
#7150=ORIENTED_EDGE('',*,*,#5325,.T.);
#7151=ORIENTED_EDGE('',*,*,#5346,.F.);
#7152=ORIENTED_EDGE('',*,*,#5320,.F.);
#7153=ORIENTED_EDGE('',*,*,#5348,.T.);
#7154=ORIENTED_EDGE('',*,*,#5318,.T.);
#7155=ORIENTED_EDGE('',*,*,#5348,.F.);
#7156=ORIENTED_EDGE('',*,*,#5324,.F.);
#7157=ORIENTED_EDGE('',*,*,#5349,.T.);
#7158=ORIENTED_EDGE('',*,*,#5279,.F.);
#7159=ORIENTED_EDGE('',*,*,#5282,.T.);
#7160=ORIENTED_EDGE('',*,*,#5285,.T.);
#7161=ORIENTED_EDGE('',*,*,#5288,.T.);
#7162=ORIENTED_EDGE('',*,*,#5313,.T.);
#7163=ORIENTED_EDGE('',*,*,#5349,.F.);
#7164=ORIENTED_EDGE('',*,*,#5306,.F.);
#7165=ORIENTED_EDGE('',*,*,#5350,.T.);
#7166=ORIENTED_EDGE('',*,*,#5351,.T.);
#7167=ORIENTED_EDGE('',*,*,#5350,.F.);
#7168=ORIENTED_EDGE('',*,*,#5311,.F.);
#7169=ORIENTED_EDGE('',*,*,#5352,.T.);
#7170=ORIENTED_EDGE('',*,*,#5291,.T.);
#7171=ORIENTED_EDGE('',*,*,#5294,.T.);
#7172=ORIENTED_EDGE('',*,*,#5297,.T.);
#7173=ORIENTED_EDGE('',*,*,#5300,.T.);
#7174=ORIENTED_EDGE('',*,*,#5353,.T.);
#7175=ORIENTED_EDGE('',*,*,#5352,.F.);
#7176=ORIENTED_EDGE('',*,*,#5310,.F.);
#7177=ORIENTED_EDGE('',*,*,#5354,.T.);
#7178=ORIENTED_EDGE('',*,*,#5355,.F.);
#7179=ORIENTED_EDGE('',*,*,#5354,.F.);
#7180=ORIENTED_EDGE('',*,*,#5309,.T.);
#7181=ORIENTED_EDGE('',*,*,#5356,.T.);
#7182=ORIENTED_EDGE('',*,*,#5289,.F.);
#7183=ORIENTED_EDGE('',*,*,#5292,.F.);
#7184=ORIENTED_EDGE('',*,*,#5295,.F.);
#7185=ORIENTED_EDGE('',*,*,#5298,.F.);
#7186=ORIENTED_EDGE('',*,*,#5315,.F.);
#7187=ORIENTED_EDGE('',*,*,#5356,.F.);
#7188=ORIENTED_EDGE('',*,*,#5308,.T.);
#7189=ORIENTED_EDGE('',*,*,#5357,.T.);
#7190=ORIENTED_EDGE('',*,*,#5316,.F.);
#7191=ORIENTED_EDGE('',*,*,#5357,.F.);
#7192=ORIENTED_EDGE('',*,*,#5323,.T.);
#7193=ORIENTED_EDGE('',*,*,#5358,.T.);
#7194=ORIENTED_EDGE('',*,*,#5277,.T.);
#7195=ORIENTED_EDGE('',*,*,#5280,.F.);
#7196=ORIENTED_EDGE('',*,*,#5283,.F.);
#7197=ORIENTED_EDGE('',*,*,#5286,.F.);
#7198=ORIENTED_EDGE('',*,*,#5326,.F.);
#7199=ORIENTED_EDGE('',*,*,#5358,.F.);
#7200=ORIENTED_EDGE('',*,*,#5322,.T.);
#7201=ORIENTED_EDGE('',*,*,#5359,.T.);
#7202=ORIENTED_EDGE('',*,*,#5360,.T.);
#7203=ORIENTED_EDGE('',*,*,#5303,.F.);
#7204=ORIENTED_EDGE('',*,*,#5359,.F.);
#7205=ORIENTED_EDGE('',*,*,#5328,.T.);
#7206=ORIENTED_EDGE('',*,*,#5361,.F.);
#7207=ORIENTED_EDGE('',*,*,#5362,.F.);
#7208=ORIENTED_EDGE('',*,*,#5363,.T.);
#7209=ORIENTED_EDGE('',*,*,#5364,.F.);
#7210=ORIENTED_EDGE('',*,*,#5363,.F.);
#7211=ORIENTED_EDGE('',*,*,#5365,.F.);
#7212=ORIENTED_EDGE('',*,*,#5330,.T.);
#7213=ORIENTED_EDGE('',*,*,#5366,.F.);
#7214=ORIENTED_EDGE('',*,*,#5351,.F.);
#7215=ORIENTED_EDGE('',*,*,#5353,.F.);
#7216=ORIENTED_EDGE('',*,*,#5355,.T.);
#7217=ORIENTED_EDGE('',*,*,#5314,.F.);
#7218=ORIENTED_EDGE('',*,*,#5345,.F.);
#7219=ORIENTED_EDGE('',*,*,#5367,.F.);
#7220=ORIENTED_EDGE('',*,*,#5361,.T.);
#7221=ORIENTED_EDGE('',*,*,#5327,.F.);
#7222=ORIENTED_EDGE('',*,*,#5341,.F.);
#7223=ORIENTED_EDGE('',*,*,#5338,.F.);
#7224=ORIENTED_EDGE('',*,*,#5335,.F.);
#7225=ORIENTED_EDGE('',*,*,#5331,.T.);
#7226=ORIENTED_EDGE('',*,*,#5365,.T.);
#7227=ORIENTED_EDGE('',*,*,#5362,.T.);
#7228=ORIENTED_EDGE('',*,*,#5367,.T.);
#7229=ORIENTED_EDGE('',*,*,#5344,.F.);
#7230=ORIENTED_EDGE('',*,*,#5340,.F.);
#7231=ORIENTED_EDGE('',*,*,#5343,.F.);
#7232=ORIENTED_EDGE('',*,*,#5368,.T.);
#7233=ORIENTED_EDGE('',*,*,#5364,.T.);
#7234=ORIENTED_EDGE('',*,*,#5366,.T.);
#7235=ORIENTED_EDGE('',*,*,#5333,.T.);
#7236=ORIENTED_EDGE('',*,*,#5334,.T.);
#7237=ORIENTED_EDGE('',*,*,#5337,.F.);
#7238=ORIENTED_EDGE('',*,*,#5368,.F.);
#7239=ORIENTED_EDGE('',*,*,#5347,.T.);
#7240=ORIENTED_EDGE('',*,*,#5304,.T.);
#7241=ORIENTED_EDGE('',*,*,#5360,.F.);
#7242=ORIENTED_EDGE('',*,*,#5369,.F.);
#7243=ORIENTED_EDGE('',*,*,#5370,.T.);
#7244=ORIENTED_EDGE('',*,*,#5371,.T.);
#7245=ORIENTED_EDGE('',*,*,#5370,.F.);
#7246=ORIENTED_EDGE('',*,*,#5372,.F.);
#7247=ORIENTED_EDGE('',*,*,#5373,.T.);
#7248=ORIENTED_EDGE('',*,*,#5374,.T.);
#7249=ORIENTED_EDGE('',*,*,#5373,.F.);
#7250=ORIENTED_EDGE('',*,*,#5375,.F.);
#7251=ORIENTED_EDGE('',*,*,#5376,.T.);
#7252=ORIENTED_EDGE('',*,*,#5377,.T.);
#7253=ORIENTED_EDGE('',*,*,#5376,.F.);
#7254=ORIENTED_EDGE('',*,*,#5378,.F.);
#7255=ORIENTED_EDGE('',*,*,#5379,.F.);
#7256=ORIENTED_EDGE('',*,*,#5380,.F.);
#7257=ORIENTED_EDGE('',*,*,#5381,.T.);
#7258=ORIENTED_EDGE('',*,*,#5382,.F.);
#7259=ORIENTED_EDGE('',*,*,#5378,.T.);
#7260=ORIENTED_EDGE('',*,*,#5383,.T.);
#7261=ORIENTED_EDGE('',*,*,#5384,.T.);
#7262=ORIENTED_EDGE('',*,*,#5385,.F.);
#7263=ORIENTED_EDGE('',*,*,#5386,.T.);
#7264=ORIENTED_EDGE('',*,*,#5387,.F.);
#7265=ORIENTED_EDGE('',*,*,#5388,.F.);
#7266=ORIENTED_EDGE('',*,*,#5389,.T.);
#7267=ORIENTED_EDGE('',*,*,#5385,.T.);
#7268=ORIENTED_EDGE('',*,*,#5390,.F.);
#7269=ORIENTED_EDGE('',*,*,#5391,.T.);
#7270=ORIENTED_EDGE('',*,*,#5392,.F.);
#7271=ORIENTED_EDGE('',*,*,#5393,.F.);
#7272=ORIENTED_EDGE('',*,*,#5384,.F.);
#7273=ORIENTED_EDGE('',*,*,#5394,.T.);
#7274=ORIENTED_EDGE('',*,*,#5395,.F.);
#7275=ORIENTED_EDGE('',*,*,#5392,.T.);
#7276=ORIENTED_EDGE('',*,*,#5396,.T.);
#7277=ORIENTED_EDGE('',*,*,#5397,.T.);
#7278=ORIENTED_EDGE('',*,*,#5398,.F.);
#7279=ORIENTED_EDGE('',*,*,#5399,.T.);
#7280=ORIENTED_EDGE('',*,*,#5400,.F.);
#7281=ORIENTED_EDGE('',*,*,#5401,.F.);
#7282=ORIENTED_EDGE('',*,*,#5402,.T.);
#7283=ORIENTED_EDGE('',*,*,#5398,.T.);
#7284=ORIENTED_EDGE('',*,*,#5403,.F.);
#7285=ORIENTED_EDGE('',*,*,#5387,.T.);
#7286=ORIENTED_EDGE('',*,*,#5404,.F.);
#7287=ORIENTED_EDGE('',*,*,#5405,.F.);
#7288=ORIENTED_EDGE('',*,*,#5397,.F.);
#7289=ORIENTED_EDGE('',*,*,#5406,.T.);
#7290=ORIENTED_EDGE('',*,*,#5407,.F.);
#7291=ORIENTED_EDGE('',*,*,#5408,.F.);
#7292=ORIENTED_EDGE('',*,*,#5404,.T.);
#7293=ORIENTED_EDGE('',*,*,#5409,.T.);
#7294=ORIENTED_EDGE('',*,*,#5410,.F.);
#7295=ORIENTED_EDGE('',*,*,#5411,.T.);
#7296=ORIENTED_EDGE('',*,*,#5412,.F.);
#7297=ORIENTED_EDGE('',*,*,#5413,.F.);
#7298=ORIENTED_EDGE('',*,*,#5414,.T.);
#7299=ORIENTED_EDGE('',*,*,#5410,.T.);
#7300=ORIENTED_EDGE('',*,*,#5415,.F.);
#7301=ORIENTED_EDGE('',*,*,#5400,.T.);
#7302=ORIENTED_EDGE('',*,*,#5416,.T.);
#7303=ORIENTED_EDGE('',*,*,#5417,.F.);
#7304=ORIENTED_EDGE('',*,*,#5412,.T.);
#7305=ORIENTED_EDGE('',*,*,#5418,.T.);
#7306=ORIENTED_EDGE('',*,*,#5419,.F.);
#7307=ORIENTED_EDGE('',*,*,#5420,.T.);
#7308=ORIENTED_EDGE('',*,*,#5421,.T.);
#7309=ORIENTED_EDGE('',*,*,#5422,.F.);
#7310=ORIENTED_EDGE('',*,*,#5423,.F.);
#7311=ORIENTED_EDGE('',*,*,#5419,.T.);
#7312=ORIENTED_EDGE('',*,*,#5424,.F.);
#7313=ORIENTED_EDGE('',*,*,#5425,.F.);
#7314=ORIENTED_EDGE('',*,*,#5426,.F.);
#7315=ORIENTED_EDGE('',*,*,#5425,.T.);
#7316=ORIENTED_EDGE('',*,*,#5427,.F.);
#7317=ORIENTED_EDGE('',*,*,#5428,.F.);
#7318=ORIENTED_EDGE('',*,*,#5429,.F.);
#7319=ORIENTED_EDGE('',*,*,#5428,.T.);
#7320=ORIENTED_EDGE('',*,*,#5430,.F.);
#7321=ORIENTED_EDGE('',*,*,#5431,.F.);
#7322=ORIENTED_EDGE('',*,*,#5432,.F.);
#7323=ORIENTED_EDGE('',*,*,#5431,.T.);
#7324=ORIENTED_EDGE('',*,*,#5433,.F.);
#7325=ORIENTED_EDGE('',*,*,#5434,.F.);
#7326=ORIENTED_EDGE('',*,*,#5418,.F.);
#7327=ORIENTED_EDGE('',*,*,#5435,.F.);
#7328=ORIENTED_EDGE('',*,*,#5408,.T.);
#7329=ORIENTED_EDGE('',*,*,#5436,.F.);
#7330=ORIENTED_EDGE('',*,*,#5411,.F.);
#7331=ORIENTED_EDGE('',*,*,#5437,.F.);
#7332=ORIENTED_EDGE('',*,*,#5405,.T.);
#7333=ORIENTED_EDGE('',*,*,#5435,.T.);
#7334=ORIENTED_EDGE('',*,*,#5414,.F.);
#7335=ORIENTED_EDGE('',*,*,#5438,.F.);
#7336=ORIENTED_EDGE('',*,*,#5395,.T.);
#7337=ORIENTED_EDGE('',*,*,#5437,.T.);
#7338=ORIENTED_EDGE('',*,*,#5399,.F.);
#7339=ORIENTED_EDGE('',*,*,#5439,.F.);
#7340=ORIENTED_EDGE('',*,*,#5393,.T.);
#7341=ORIENTED_EDGE('',*,*,#5438,.T.);
#7342=ORIENTED_EDGE('',*,*,#5402,.F.);
#7343=ORIENTED_EDGE('',*,*,#5440,.F.);
#7344=ORIENTED_EDGE('',*,*,#5382,.T.);
#7345=ORIENTED_EDGE('',*,*,#5439,.T.);
#7346=ORIENTED_EDGE('',*,*,#5386,.F.);
#7347=ORIENTED_EDGE('',*,*,#5441,.F.);
#7348=ORIENTED_EDGE('',*,*,#5379,.T.);
#7349=ORIENTED_EDGE('',*,*,#5440,.T.);
#7350=ORIENTED_EDGE('',*,*,#5389,.F.);
#7351=ORIENTED_EDGE('',*,*,#5442,.F.);
#7352=ORIENTED_EDGE('',*,*,#5443,.T.);
#7353=ORIENTED_EDGE('',*,*,#5441,.T.);
#7354=ORIENTED_EDGE('',*,*,#5371,.F.);
#7355=ORIENTED_EDGE('',*,*,#5374,.F.);
#7356=ORIENTED_EDGE('',*,*,#5377,.F.);
#7357=ORIENTED_EDGE('',*,*,#5391,.F.);
#7358=ORIENTED_EDGE('',*,*,#5444,.F.);
#7359=ORIENTED_EDGE('',*,*,#5445,.T.);
#7360=ORIENTED_EDGE('',*,*,#5442,.T.);
#7361=ORIENTED_EDGE('',*,*,#5390,.T.);
#7362=ORIENTED_EDGE('',*,*,#5446,.F.);
#7363=ORIENTED_EDGE('',*,*,#5447,.F.);
#7364=ORIENTED_EDGE('',*,*,#5444,.T.);
#7365=ORIENTED_EDGE('',*,*,#5369,.T.);
#7366=ORIENTED_EDGE('',*,*,#5372,.T.);
#7367=ORIENTED_EDGE('',*,*,#5375,.T.);
#7368=ORIENTED_EDGE('',*,*,#5388,.T.);
#7369=ORIENTED_EDGE('',*,*,#5448,.F.);
#7370=ORIENTED_EDGE('',*,*,#5381,.F.);
#7371=ORIENTED_EDGE('',*,*,#5446,.T.);
#7372=ORIENTED_EDGE('',*,*,#5403,.T.);
#7373=ORIENTED_EDGE('',*,*,#5449,.F.);
#7374=ORIENTED_EDGE('',*,*,#5383,.F.);
#7375=ORIENTED_EDGE('',*,*,#5448,.T.);
#7376=ORIENTED_EDGE('',*,*,#5401,.T.);
#7377=ORIENTED_EDGE('',*,*,#5450,.F.);
#7378=ORIENTED_EDGE('',*,*,#5394,.F.);
#7379=ORIENTED_EDGE('',*,*,#5449,.T.);
#7380=ORIENTED_EDGE('',*,*,#5415,.T.);
#7381=ORIENTED_EDGE('',*,*,#5451,.F.);
#7382=ORIENTED_EDGE('',*,*,#5396,.F.);
#7383=ORIENTED_EDGE('',*,*,#5450,.T.);
#7384=ORIENTED_EDGE('',*,*,#5413,.T.);
#7385=ORIENTED_EDGE('',*,*,#5452,.F.);
#7386=ORIENTED_EDGE('',*,*,#5406,.F.);
#7387=ORIENTED_EDGE('',*,*,#5451,.T.);
#7388=ORIENTED_EDGE('',*,*,#5453,.F.);
#7389=ORIENTED_EDGE('',*,*,#5454,.F.);
#7390=ORIENTED_EDGE('',*,*,#5455,.F.);
#7391=ORIENTED_EDGE('',*,*,#5409,.F.);
#7392=ORIENTED_EDGE('',*,*,#5452,.T.);
#7393=ORIENTED_EDGE('',*,*,#5417,.T.);
#7394=ORIENTED_EDGE('',*,*,#5456,.F.);
#7395=ORIENTED_EDGE('',*,*,#5457,.F.);
#7396=ORIENTED_EDGE('',*,*,#5421,.F.);
#7397=ORIENTED_EDGE('',*,*,#5458,.T.);
#7398=ORIENTED_EDGE('',*,*,#5453,.T.);
#7399=ORIENTED_EDGE('',*,*,#5459,.T.);
#7400=ORIENTED_EDGE('',*,*,#5447,.T.);
#7401=ORIENTED_EDGE('',*,*,#5380,.T.);
#7402=ORIENTED_EDGE('',*,*,#5443,.F.);
#7403=ORIENTED_EDGE('',*,*,#5445,.F.);
#7404=ORIENTED_EDGE('',*,*,#5424,.T.);
#7405=ORIENTED_EDGE('',*,*,#5422,.T.);
#7406=ORIENTED_EDGE('',*,*,#5459,.F.);
#7407=ORIENTED_EDGE('',*,*,#5457,.T.);
#7408=ORIENTED_EDGE('',*,*,#5460,.F.);
#7409=ORIENTED_EDGE('',*,*,#5433,.T.);
#7410=ORIENTED_EDGE('',*,*,#5430,.T.);
#7411=ORIENTED_EDGE('',*,*,#5427,.T.);
#7412=ORIENTED_EDGE('',*,*,#5434,.T.);
#7413=ORIENTED_EDGE('',*,*,#5460,.T.);
#7414=ORIENTED_EDGE('',*,*,#5456,.T.);
#7415=ORIENTED_EDGE('',*,*,#5416,.F.);
#7416=ORIENTED_EDGE('',*,*,#5423,.T.);
#7417=ORIENTED_EDGE('',*,*,#5426,.T.);
#7418=ORIENTED_EDGE('',*,*,#5429,.T.);
#7419=ORIENTED_EDGE('',*,*,#5432,.T.);
#7420=ORIENTED_EDGE('',*,*,#5461,.T.);
#7421=ORIENTED_EDGE('',*,*,#5454,.T.);
#7422=ORIENTED_EDGE('',*,*,#5458,.F.);
#7423=ORIENTED_EDGE('',*,*,#5420,.F.);
#7424=ORIENTED_EDGE('',*,*,#5436,.T.);
#7425=ORIENTED_EDGE('',*,*,#5407,.T.);
#7426=ORIENTED_EDGE('',*,*,#5455,.T.);
#7427=ORIENTED_EDGE('',*,*,#5461,.F.);
#7428=ORIENTED_EDGE('',*,*,#5462,.F.);
#7429=ORIENTED_EDGE('',*,*,#5463,.F.);
#7430=ORIENTED_EDGE('',*,*,#5464,.F.);
#7431=ORIENTED_EDGE('',*,*,#5465,.T.);
#7432=ORIENTED_EDGE('',*,*,#5466,.F.);
#7433=ORIENTED_EDGE('',*,*,#5462,.T.);
#7434=ORIENTED_EDGE('',*,*,#5467,.T.);
#7435=ORIENTED_EDGE('',*,*,#5468,.T.);
#7436=ORIENTED_EDGE('',*,*,#5469,.F.);
#7437=ORIENTED_EDGE('',*,*,#5470,.T.);
#7438=ORIENTED_EDGE('',*,*,#5471,.F.);
#7439=ORIENTED_EDGE('',*,*,#5472,.F.);
#7440=ORIENTED_EDGE('',*,*,#5473,.T.);
#7441=ORIENTED_EDGE('',*,*,#5469,.T.);
#7442=ORIENTED_EDGE('',*,*,#5474,.F.);
#7443=ORIENTED_EDGE('',*,*,#5475,.T.);
#7444=ORIENTED_EDGE('',*,*,#5476,.F.);
#7445=ORIENTED_EDGE('',*,*,#5477,.F.);
#7446=ORIENTED_EDGE('',*,*,#5468,.F.);
#7447=ORIENTED_EDGE('',*,*,#5478,.T.);
#7448=ORIENTED_EDGE('',*,*,#5479,.F.);
#7449=ORIENTED_EDGE('',*,*,#5476,.T.);
#7450=ORIENTED_EDGE('',*,*,#5480,.T.);
#7451=ORIENTED_EDGE('',*,*,#5481,.F.);
#7452=ORIENTED_EDGE('',*,*,#5482,.F.);
#7453=ORIENTED_EDGE('',*,*,#5483,.T.);
#7454=ORIENTED_EDGE('',*,*,#5484,.F.);
#7455=ORIENTED_EDGE('',*,*,#5485,.F.);
#7456=ORIENTED_EDGE('',*,*,#5486,.T.);
#7457=ORIENTED_EDGE('',*,*,#5482,.T.);
#7458=ORIENTED_EDGE('',*,*,#5487,.F.);
#7459=ORIENTED_EDGE('',*,*,#5471,.T.);
#7460=ORIENTED_EDGE('',*,*,#5488,.T.);
#7461=ORIENTED_EDGE('',*,*,#5489,.F.);
#7462=ORIENTED_EDGE('',*,*,#5480,.F.);
#7463=ORIENTED_EDGE('',*,*,#5490,.T.);
#7464=ORIENTED_EDGE('',*,*,#5491,.F.);
#7465=ORIENTED_EDGE('',*,*,#5492,.F.);
#7466=ORIENTED_EDGE('',*,*,#5481,.T.);
#7467=ORIENTED_EDGE('',*,*,#5489,.T.);
#7468=ORIENTED_EDGE('',*,*,#5493,.F.);
#7469=ORIENTED_EDGE('',*,*,#5494,.F.);
#7470=ORIENTED_EDGE('',*,*,#5479,.T.);
#7471=ORIENTED_EDGE('',*,*,#5492,.T.);
#7472=ORIENTED_EDGE('',*,*,#5483,.F.);
#7473=ORIENTED_EDGE('',*,*,#5495,.F.);
#7474=ORIENTED_EDGE('',*,*,#5477,.T.);
#7475=ORIENTED_EDGE('',*,*,#5494,.T.);
#7476=ORIENTED_EDGE('',*,*,#5486,.F.);
#7477=ORIENTED_EDGE('',*,*,#5496,.F.);
#7478=ORIENTED_EDGE('',*,*,#5466,.T.);
#7479=ORIENTED_EDGE('',*,*,#5495,.T.);
#7480=ORIENTED_EDGE('',*,*,#5470,.F.);
#7481=ORIENTED_EDGE('',*,*,#5497,.F.);
#7482=ORIENTED_EDGE('',*,*,#5463,.T.);
#7483=ORIENTED_EDGE('',*,*,#5496,.T.);
#7484=ORIENTED_EDGE('',*,*,#5473,.F.);
#7485=ORIENTED_EDGE('',*,*,#5498,.F.);
#7486=ORIENTED_EDGE('',*,*,#5499,.T.);
#7487=ORIENTED_EDGE('',*,*,#5497,.T.);
#7488=ORIENTED_EDGE('',*,*,#5475,.F.);
#7489=ORIENTED_EDGE('',*,*,#5500,.F.);
#7490=ORIENTED_EDGE('',*,*,#5501,.T.);
#7491=ORIENTED_EDGE('',*,*,#5498,.T.);
#7492=ORIENTED_EDGE('',*,*,#5474,.T.);
#7493=ORIENTED_EDGE('',*,*,#5502,.F.);
#7494=ORIENTED_EDGE('',*,*,#5503,.F.);
#7495=ORIENTED_EDGE('',*,*,#5500,.T.);
#7496=ORIENTED_EDGE('',*,*,#5472,.T.);
#7497=ORIENTED_EDGE('',*,*,#5504,.F.);
#7498=ORIENTED_EDGE('',*,*,#5465,.F.);
#7499=ORIENTED_EDGE('',*,*,#5502,.T.);
#7500=ORIENTED_EDGE('',*,*,#5487,.T.);
#7501=ORIENTED_EDGE('',*,*,#5505,.F.);
#7502=ORIENTED_EDGE('',*,*,#5467,.F.);
#7503=ORIENTED_EDGE('',*,*,#5504,.T.);
#7504=ORIENTED_EDGE('',*,*,#5485,.T.);
#7505=ORIENTED_EDGE('',*,*,#5490,.F.);
#7506=ORIENTED_EDGE('',*,*,#5478,.F.);
#7507=ORIENTED_EDGE('',*,*,#5505,.T.);
#7508=ORIENTED_EDGE('',*,*,#5503,.T.);
#7509=ORIENTED_EDGE('',*,*,#5464,.T.);
#7510=ORIENTED_EDGE('',*,*,#5499,.F.);
#7511=ORIENTED_EDGE('',*,*,#5501,.F.);
#7512=ORIENTED_EDGE('',*,*,#5488,.F.);
#7513=ORIENTED_EDGE('',*,*,#5484,.T.);
#7514=ORIENTED_EDGE('',*,*,#5493,.T.);
#7515=ORIENTED_EDGE('',*,*,#5491,.T.);
#7516=ORIENTED_EDGE('',*,*,#5506,.T.);
#7517=ORIENTED_EDGE('',*,*,#5507,.T.);
#7518=ORIENTED_EDGE('',*,*,#5508,.F.);
#7519=ORIENTED_EDGE('',*,*,#5509,.T.);
#7520=ORIENTED_EDGE('',*,*,#5510,.T.);
#7521=ORIENTED_EDGE('',*,*,#5511,.F.);
#7522=ORIENTED_EDGE('',*,*,#5508,.T.);
#7523=ORIENTED_EDGE('',*,*,#5512,.F.);
#7524=ORIENTED_EDGE('',*,*,#5513,.F.);
#7525=ORIENTED_EDGE('',*,*,#5514,.F.);
#7526=ORIENTED_EDGE('',*,*,#5515,.F.);
#7527=ORIENTED_EDGE('',*,*,#5516,.F.);
#7528=ORIENTED_EDGE('',*,*,#5517,.T.);
#7529=ORIENTED_EDGE('',*,*,#5518,.F.);
#7530=ORIENTED_EDGE('',*,*,#5519,.T.);
#7531=ORIENTED_EDGE('',*,*,#5520,.F.);
#7532=ORIENTED_EDGE('',*,*,#5521,.F.);
#7533=ORIENTED_EDGE('',*,*,#5522,.F.);
#7534=ORIENTED_EDGE('',*,*,#5523,.F.);
#7535=ORIENTED_EDGE('',*,*,#5524,.F.);
#7536=ORIENTED_EDGE('',*,*,#5525,.F.);
#7537=ORIENTED_EDGE('',*,*,#5526,.F.);
#7538=ORIENTED_EDGE('',*,*,#5527,.F.);
#7539=ORIENTED_EDGE('',*,*,#5528,.F.);
#7540=ORIENTED_EDGE('',*,*,#5529,.F.);
#7541=ORIENTED_EDGE('',*,*,#5530,.F.);
#7542=ORIENTED_EDGE('',*,*,#5531,.F.);
#7543=ORIENTED_EDGE('',*,*,#5532,.F.);
#7544=ORIENTED_EDGE('',*,*,#5533,.F.);
#7545=ORIENTED_EDGE('',*,*,#5534,.F.);
#7546=ORIENTED_EDGE('',*,*,#5535,.F.);
#7547=ORIENTED_EDGE('',*,*,#5536,.F.);
#7548=ORIENTED_EDGE('',*,*,#5537,.F.);
#7549=ORIENTED_EDGE('',*,*,#5538,.F.);
#7550=ORIENTED_EDGE('',*,*,#5539,.T.);
#7551=ORIENTED_EDGE('',*,*,#5540,.F.);
#7552=ORIENTED_EDGE('',*,*,#5541,.T.);
#7553=ORIENTED_EDGE('',*,*,#5542,.F.);
#7554=ORIENTED_EDGE('',*,*,#5543,.T.);
#7555=ORIENTED_EDGE('',*,*,#5544,.F.);
#7556=ORIENTED_EDGE('',*,*,#5545,.T.);
#7557=ORIENTED_EDGE('',*,*,#5546,.F.);
#7558=ORIENTED_EDGE('',*,*,#5547,.F.);
#7559=ORIENTED_EDGE('',*,*,#5548,.F.);
#7560=ORIENTED_EDGE('',*,*,#5549,.F.);
#7561=ORIENTED_EDGE('',*,*,#5550,.F.);
#7562=ORIENTED_EDGE('',*,*,#5551,.F.);
#7563=ORIENTED_EDGE('',*,*,#5552,.F.);
#7564=ORIENTED_EDGE('',*,*,#5553,.F.);
#7565=ORIENTED_EDGE('',*,*,#5554,.F.);
#7566=ORIENTED_EDGE('',*,*,#5555,.F.);
#7567=ORIENTED_EDGE('',*,*,#5556,.F.);
#7568=ORIENTED_EDGE('',*,*,#5557,.F.);
#7569=ORIENTED_EDGE('',*,*,#5558,.F.);
#7570=ORIENTED_EDGE('',*,*,#5559,.F.);
#7571=ORIENTED_EDGE('',*,*,#5560,.F.);
#7572=ORIENTED_EDGE('',*,*,#5561,.F.);
#7573=ORIENTED_EDGE('',*,*,#5562,.F.);
#7574=ORIENTED_EDGE('',*,*,#5563,.F.);
#7575=ORIENTED_EDGE('',*,*,#5564,.F.);
#7576=ORIENTED_EDGE('',*,*,#5565,.F.);
#7577=ORIENTED_EDGE('',*,*,#5566,.F.);
#7578=ORIENTED_EDGE('',*,*,#5567,.F.);
#7579=ORIENTED_EDGE('',*,*,#5568,.F.);
#7580=ORIENTED_EDGE('',*,*,#5569,.F.);
#7581=ORIENTED_EDGE('',*,*,#5570,.F.);
#7582=ORIENTED_EDGE('',*,*,#5571,.F.);
#7583=ORIENTED_EDGE('',*,*,#5572,.F.);
#7584=ORIENTED_EDGE('',*,*,#5573,.F.);
#7585=ORIENTED_EDGE('',*,*,#5574,.F.);
#7586=ORIENTED_EDGE('',*,*,#5575,.T.);
#7587=ORIENTED_EDGE('',*,*,#5576,.F.);
#7588=ORIENTED_EDGE('',*,*,#5577,.T.);
#7589=ORIENTED_EDGE('',*,*,#5578,.F.);
#7590=ORIENTED_EDGE('',*,*,#5579,.T.);
#7591=ORIENTED_EDGE('',*,*,#5580,.F.);
#7592=ORIENTED_EDGE('',*,*,#5581,.F.);
#7593=ORIENTED_EDGE('',*,*,#5582,.F.);
#7594=ORIENTED_EDGE('',*,*,#5583,.F.);
#7595=ORIENTED_EDGE('',*,*,#5584,.F.);
#7596=ORIENTED_EDGE('',*,*,#5585,.F.);
#7597=ORIENTED_EDGE('',*,*,#5586,.F.);
#7598=ORIENTED_EDGE('',*,*,#5587,.F.);
#7599=ORIENTED_EDGE('',*,*,#5588,.F.);
#7600=ORIENTED_EDGE('',*,*,#5589,.T.);
#7601=ORIENTED_EDGE('',*,*,#5590,.F.);
#7602=ORIENTED_EDGE('',*,*,#5591,.T.);
#7603=ORIENTED_EDGE('',*,*,#5592,.F.);
#7604=ORIENTED_EDGE('',*,*,#5593,.T.);
#7605=ORIENTED_EDGE('',*,*,#5594,.F.);
#7606=ORIENTED_EDGE('',*,*,#5531,.T.);
#7607=ORIENTED_EDGE('',*,*,#5595,.T.);
#7608=ORIENTED_EDGE('',*,*,#5596,.T.);
#7609=ORIENTED_EDGE('',*,*,#5597,.F.);
#7610=ORIENTED_EDGE('',*,*,#5598,.F.);
#7611=ORIENTED_EDGE('',*,*,#5599,.T.);
#7612=ORIENTED_EDGE('',*,*,#5600,.F.);
#7613=ORIENTED_EDGE('',*,*,#5601,.F.);
#7614=ORIENTED_EDGE('',*,*,#5551,.T.);
#7615=ORIENTED_EDGE('',*,*,#5602,.T.);
#7616=ORIENTED_EDGE('',*,*,#5603,.T.);
#7617=ORIENTED_EDGE('',*,*,#5604,.F.);
#7618=ORIENTED_EDGE('',*,*,#5543,.F.);
#7619=ORIENTED_EDGE('',*,*,#5605,.T.);
#7620=ORIENTED_EDGE('',*,*,#5606,.F.);
#7621=ORIENTED_EDGE('',*,*,#5607,.F.);
#7622=ORIENTED_EDGE('',*,*,#5608,.F.);
#7623=ORIENTED_EDGE('',*,*,#5609,.T.);
#7624=ORIENTED_EDGE('',*,*,#5610,.F.);
#7625=ORIENTED_EDGE('',*,*,#5611,.F.);
#7626=ORIENTED_EDGE('',*,*,#5563,.T.);
#7627=ORIENTED_EDGE('',*,*,#5612,.T.);
#7628=ORIENTED_EDGE('',*,*,#5613,.T.);
#7629=ORIENTED_EDGE('',*,*,#5614,.F.);
#7630=ORIENTED_EDGE('',*,*,#5585,.T.);
#7631=ORIENTED_EDGE('',*,*,#5615,.T.);
#7632=ORIENTED_EDGE('',*,*,#5616,.T.);
#7633=ORIENTED_EDGE('',*,*,#5617,.F.);
#7634=ORIENTED_EDGE('',*,*,#5579,.F.);
#7635=ORIENTED_EDGE('',*,*,#5618,.T.);
#7636=ORIENTED_EDGE('',*,*,#5619,.F.);
#7637=ORIENTED_EDGE('',*,*,#5620,.F.);
#7638=ORIENTED_EDGE('',*,*,#5567,.T.);
#7639=ORIENTED_EDGE('',*,*,#5621,.T.);
#7640=ORIENTED_EDGE('',*,*,#5622,.T.);
#7641=ORIENTED_EDGE('',*,*,#5623,.F.);
#7642=ORIENTED_EDGE('',*,*,#5589,.F.);
#7643=ORIENTED_EDGE('',*,*,#5624,.T.);
#7644=ORIENTED_EDGE('',*,*,#5625,.F.);
#7645=ORIENTED_EDGE('',*,*,#5626,.F.);
#7646=ORIENTED_EDGE('',*,*,#5627,.F.);
#7647=ORIENTED_EDGE('',*,*,#5628,.T.);
#7648=ORIENTED_EDGE('',*,*,#5629,.T.);
#7649=ORIENTED_EDGE('',*,*,#5628,.F.);
#7650=ORIENTED_EDGE('',*,*,#5630,.F.);
#7651=ORIENTED_EDGE('',*,*,#5631,.T.);
#7652=ORIENTED_EDGE('',*,*,#5632,.T.);
#7653=ORIENTED_EDGE('',*,*,#5633,.T.);
#7654=ORIENTED_EDGE('',*,*,#5632,.F.);
#7655=ORIENTED_EDGE('',*,*,#5634,.F.);
#7656=ORIENTED_EDGE('',*,*,#5635,.F.);
#7657=ORIENTED_EDGE('',*,*,#5636,.F.);
#7658=ORIENTED_EDGE('',*,*,#5637,.T.);
#7659=ORIENTED_EDGE('',*,*,#5638,.T.);
#7660=ORIENTED_EDGE('',*,*,#5639,.F.);
#7661=ORIENTED_EDGE('',*,*,#5638,.F.);
#7662=ORIENTED_EDGE('',*,*,#5640,.F.);
#7663=ORIENTED_EDGE('',*,*,#5641,.T.);
#7664=ORIENTED_EDGE('',*,*,#5642,.T.);
#7665=ORIENTED_EDGE('',*,*,#5641,.F.);
#7666=ORIENTED_EDGE('',*,*,#5510,.F.);
#7667=ORIENTED_EDGE('',*,*,#5643,.F.);
#7668=ORIENTED_EDGE('',*,*,#5644,.F.);
#7669=ORIENTED_EDGE('',*,*,#5645,.T.);
#7670=ORIENTED_EDGE('',*,*,#5635,.T.);
#7671=ORIENTED_EDGE('',*,*,#5646,.T.);
#7672=ORIENTED_EDGE('',*,*,#5647,.F.);
#7673=ORIENTED_EDGE('',*,*,#5648,.F.);
#7674=ORIENTED_EDGE('',*,*,#5649,.T.);
#7675=ORIENTED_EDGE('',*,*,#5650,.T.);
#7676=ORIENTED_EDGE('',*,*,#5651,.T.);
#7677=ORIENTED_EDGE('',*,*,#5652,.T.);
#7678=ORIENTED_EDGE('',*,*,#5653,.T.);
#7679=ORIENTED_EDGE('',*,*,#5654,.T.);
#7680=ORIENTED_EDGE('',*,*,#5655,.T.);
#7681=ORIENTED_EDGE('',*,*,#5656,.F.);
#7682=ORIENTED_EDGE('',*,*,#5657,.F.);
#7683=ORIENTED_EDGE('',*,*,#5658,.F.);
#7684=ORIENTED_EDGE('',*,*,#5659,.F.);
#7685=ORIENTED_EDGE('',*,*,#5660,.F.);
#7686=ORIENTED_EDGE('',*,*,#5661,.T.);
#7687=ORIENTED_EDGE('',*,*,#5644,.T.);
#7688=ORIENTED_EDGE('',*,*,#5662,.F.);
#7689=ORIENTED_EDGE('',*,*,#5655,.F.);
#7690=ORIENTED_EDGE('',*,*,#5663,.T.);
#7691=ORIENTED_EDGE('',*,*,#5649,.F.);
#7692=ORIENTED_EDGE('',*,*,#5664,.F.);
#7693=ORIENTED_EDGE('',*,*,#5647,.T.);
#7694=ORIENTED_EDGE('',*,*,#5652,.F.);
#7695=ORIENTED_EDGE('',*,*,#5665,.T.);
#7696=ORIENTED_EDGE('',*,*,#5630,.T.);
#7697=ORIENTED_EDGE('',*,*,#5666,.F.);
#7698=ORIENTED_EDGE('',*,*,#5629,.F.);
#7699=ORIENTED_EDGE('',*,*,#5653,.F.);
#7700=ORIENTED_EDGE('',*,*,#5666,.T.);
#7701=ORIENTED_EDGE('',*,*,#5633,.F.);
#7702=ORIENTED_EDGE('',*,*,#5667,.F.);
#7703=ORIENTED_EDGE('',*,*,#5651,.F.);
#7704=ORIENTED_EDGE('',*,*,#5668,.T.);
#7705=ORIENTED_EDGE('',*,*,#5631,.F.);
#7706=ORIENTED_EDGE('',*,*,#5665,.F.);
#7707=ORIENTED_EDGE('',*,*,#5669,.F.);
#7708=ORIENTED_EDGE('',*,*,#5657,.T.);
#7709=ORIENTED_EDGE('',*,*,#5670,.T.);
#7710=ORIENTED_EDGE('',*,*,#5507,.F.);
#7711=ORIENTED_EDGE('',*,*,#5671,.F.);
#7712=ORIENTED_EDGE('',*,*,#5659,.T.);
#7713=ORIENTED_EDGE('',*,*,#5672,.T.);
#7714=ORIENTED_EDGE('',*,*,#5509,.F.);
#7715=ORIENTED_EDGE('',*,*,#5670,.F.);
#7716=ORIENTED_EDGE('',*,*,#5656,.T.);
#7717=ORIENTED_EDGE('',*,*,#5662,.T.);
#7718=ORIENTED_EDGE('',*,*,#5643,.T.);
#7719=ORIENTED_EDGE('',*,*,#5512,.T.);
#7720=ORIENTED_EDGE('',*,*,#5637,.F.);
#7721=ORIENTED_EDGE('',*,*,#5664,.T.);
#7722=ORIENTED_EDGE('',*,*,#5660,.T.);
#7723=ORIENTED_EDGE('',*,*,#5671,.T.);
#7724=ORIENTED_EDGE('',*,*,#5511,.T.);
#7725=ORIENTED_EDGE('',*,*,#5648,.T.);
#7726=ORIENTED_EDGE('',*,*,#5642,.F.);
#7727=ORIENTED_EDGE('',*,*,#5672,.F.);
#7728=ORIENTED_EDGE('',*,*,#5658,.T.);
#7729=ORIENTED_EDGE('',*,*,#5669,.T.);
#7730=ORIENTED_EDGE('',*,*,#5506,.F.);
#7731=ORIENTED_EDGE('',*,*,#5627,.T.);
#7732=ORIENTED_EDGE('',*,*,#5591,.F.);
#7733=ORIENTED_EDGE('',*,*,#5673,.T.);
#7734=ORIENTED_EDGE('',*,*,#5674,.F.);
#7735=ORIENTED_EDGE('',*,*,#5675,.F.);
#7736=ORIENTED_EDGE('',*,*,#5673,.F.);
#7737=ORIENTED_EDGE('',*,*,#5590,.T.);
#7738=ORIENTED_EDGE('',*,*,#5626,.T.);
#7739=ORIENTED_EDGE('',*,*,#5676,.T.);
#7740=ORIENTED_EDGE('',*,*,#5593,.F.);
#7741=ORIENTED_EDGE('',*,*,#5677,.T.);
#7742=ORIENTED_EDGE('',*,*,#5678,.F.);
#7743=ORIENTED_EDGE('',*,*,#5679,.F.);
#7744=ORIENTED_EDGE('',*,*,#5677,.F.);
#7745=ORIENTED_EDGE('',*,*,#5592,.T.);
#7746=ORIENTED_EDGE('',*,*,#5675,.T.);
#7747=ORIENTED_EDGE('',*,*,#5680,.T.);
#7748=ORIENTED_EDGE('',*,*,#5681,.F.);
#7749=ORIENTED_EDGE('',*,*,#5569,.T.);
#7750=ORIENTED_EDGE('',*,*,#5682,.T.);
#7751=ORIENTED_EDGE('',*,*,#5683,.T.);
#7752=ORIENTED_EDGE('',*,*,#5684,.F.);
#7753=ORIENTED_EDGE('',*,*,#5571,.T.);
#7754=ORIENTED_EDGE('',*,*,#5685,.T.);
#7755=ORIENTED_EDGE('',*,*,#5686,.T.);
#7756=ORIENTED_EDGE('',*,*,#5575,.F.);
#7757=ORIENTED_EDGE('',*,*,#5687,.T.);
#7758=ORIENTED_EDGE('',*,*,#5688,.F.);
#7759=ORIENTED_EDGE('',*,*,#5689,.F.);
#7760=ORIENTED_EDGE('',*,*,#5690,.F.);
#7761=ORIENTED_EDGE('',*,*,#5572,.T.);
#7762=ORIENTED_EDGE('',*,*,#5684,.T.);
#7763=ORIENTED_EDGE('',*,*,#5691,.T.);
#7764=ORIENTED_EDGE('',*,*,#5692,.F.);
#7765=ORIENTED_EDGE('',*,*,#5573,.T.);
#7766=ORIENTED_EDGE('',*,*,#5690,.T.);
#7767=ORIENTED_EDGE('',*,*,#5693,.T.);
#7768=ORIENTED_EDGE('',*,*,#5687,.F.);
#7769=ORIENTED_EDGE('',*,*,#5574,.T.);
#7770=ORIENTED_EDGE('',*,*,#5692,.T.);
#7771=ORIENTED_EDGE('',*,*,#5694,.T.);
#7772=ORIENTED_EDGE('',*,*,#5577,.F.);
#7773=ORIENTED_EDGE('',*,*,#5695,.T.);
#7774=ORIENTED_EDGE('',*,*,#5696,.F.);
#7775=ORIENTED_EDGE('',*,*,#5697,.F.);
#7776=ORIENTED_EDGE('',*,*,#5695,.F.);
#7777=ORIENTED_EDGE('',*,*,#5576,.T.);
#7778=ORIENTED_EDGE('',*,*,#5689,.T.);
#7779=ORIENTED_EDGE('',*,*,#5698,.T.);
#7780=ORIENTED_EDGE('',*,*,#5618,.F.);
#7781=ORIENTED_EDGE('',*,*,#5578,.T.);
#7782=ORIENTED_EDGE('',*,*,#5697,.T.);
#7783=ORIENTED_EDGE('',*,*,#5699,.T.);
#7784=ORIENTED_EDGE('',*,*,#5700,.F.);
#7785=ORIENTED_EDGE('',*,*,#5581,.T.);
#7786=ORIENTED_EDGE('',*,*,#5701,.T.);
#7787=ORIENTED_EDGE('',*,*,#5702,.T.);
#7788=ORIENTED_EDGE('',*,*,#5703,.F.);
#7789=ORIENTED_EDGE('',*,*,#5583,.T.);
#7790=ORIENTED_EDGE('',*,*,#5704,.T.);
#7791=ORIENTED_EDGE('',*,*,#5705,.T.);
#7792=ORIENTED_EDGE('',*,*,#5706,.F.);
#7793=ORIENTED_EDGE('',*,*,#5586,.T.);
#7794=ORIENTED_EDGE('',*,*,#5617,.T.);
#7795=ORIENTED_EDGE('',*,*,#5707,.T.);
#7796=ORIENTED_EDGE('',*,*,#5708,.F.);
#7797=ORIENTED_EDGE('',*,*,#5587,.T.);
#7798=ORIENTED_EDGE('',*,*,#5706,.T.);
#7799=ORIENTED_EDGE('',*,*,#5709,.T.);
#7800=ORIENTED_EDGE('',*,*,#5624,.F.);
#7801=ORIENTED_EDGE('',*,*,#5588,.T.);
#7802=ORIENTED_EDGE('',*,*,#5708,.T.);
#7803=ORIENTED_EDGE('',*,*,#5710,.T.);
#7804=ORIENTED_EDGE('',*,*,#5615,.F.);
#7805=ORIENTED_EDGE('',*,*,#5584,.T.);
#7806=ORIENTED_EDGE('',*,*,#5703,.T.);
#7807=ORIENTED_EDGE('',*,*,#5711,.T.);
#7808=ORIENTED_EDGE('',*,*,#5704,.F.);
#7809=ORIENTED_EDGE('',*,*,#5582,.T.);
#7810=ORIENTED_EDGE('',*,*,#5700,.T.);
#7811=ORIENTED_EDGE('',*,*,#5712,.T.);
#7812=ORIENTED_EDGE('',*,*,#5701,.F.);
#7813=ORIENTED_EDGE('',*,*,#5580,.T.);
#7814=ORIENTED_EDGE('',*,*,#5620,.T.);
#7815=ORIENTED_EDGE('',*,*,#5713,.T.);
#7816=ORIENTED_EDGE('',*,*,#5685,.F.);
#7817=ORIENTED_EDGE('',*,*,#5570,.T.);
#7818=ORIENTED_EDGE('',*,*,#5681,.T.);
#7819=ORIENTED_EDGE('',*,*,#5714,.T.);
#7820=ORIENTED_EDGE('',*,*,#5682,.F.);
#7821=ORIENTED_EDGE('',*,*,#5568,.T.);
#7822=ORIENTED_EDGE('',*,*,#5623,.T.);
#7823=ORIENTED_EDGE('',*,*,#5715,.T.);
#7824=ORIENTED_EDGE('',*,*,#5621,.F.);
#7825=ORIENTED_EDGE('',*,*,#5594,.T.);
#7826=ORIENTED_EDGE('',*,*,#5679,.T.);
#7827=ORIENTED_EDGE('',*,*,#5716,.T.);
#7828=ORIENTED_EDGE('',*,*,#5707,.F.);
#7829=ORIENTED_EDGE('',*,*,#5616,.F.);
#7830=ORIENTED_EDGE('',*,*,#5711,.F.);
#7831=ORIENTED_EDGE('',*,*,#5705,.F.);
#7832=ORIENTED_EDGE('',*,*,#5712,.F.);
#7833=ORIENTED_EDGE('',*,*,#5702,.F.);
#7834=ORIENTED_EDGE('',*,*,#5713,.F.);
#7835=ORIENTED_EDGE('',*,*,#5619,.T.);
#7836=ORIENTED_EDGE('',*,*,#5699,.F.);
#7837=ORIENTED_EDGE('',*,*,#5696,.T.);
#7838=ORIENTED_EDGE('',*,*,#5698,.F.);
#7839=ORIENTED_EDGE('',*,*,#5688,.T.);
#7840=ORIENTED_EDGE('',*,*,#5694,.F.);
#7841=ORIENTED_EDGE('',*,*,#5693,.F.);
#7842=ORIENTED_EDGE('',*,*,#5691,.F.);
#7843=ORIENTED_EDGE('',*,*,#5686,.F.);
#7844=ORIENTED_EDGE('',*,*,#5714,.F.);
#7845=ORIENTED_EDGE('',*,*,#5683,.F.);
#7846=ORIENTED_EDGE('',*,*,#5715,.F.);
#7847=ORIENTED_EDGE('',*,*,#5622,.F.);
#7848=ORIENTED_EDGE('',*,*,#5716,.F.);
#7849=ORIENTED_EDGE('',*,*,#5678,.T.);
#7850=ORIENTED_EDGE('',*,*,#5680,.F.);
#7851=ORIENTED_EDGE('',*,*,#5674,.T.);
#7852=ORIENTED_EDGE('',*,*,#5676,.F.);
#7853=ORIENTED_EDGE('',*,*,#5625,.T.);
#7854=ORIENTED_EDGE('',*,*,#5710,.F.);
#7855=ORIENTED_EDGE('',*,*,#5709,.F.);
#7856=ORIENTED_EDGE('',*,*,#5717,.F.);
#7857=ORIENTED_EDGE('',*,*,#5565,.T.);
#7858=ORIENTED_EDGE('',*,*,#5718,.T.);
#7859=ORIENTED_EDGE('',*,*,#5719,.T.);
#7860=ORIENTED_EDGE('',*,*,#5720,.F.);
#7861=ORIENTED_EDGE('',*,*,#5559,.T.);
#7862=ORIENTED_EDGE('',*,*,#5721,.T.);
#7863=ORIENTED_EDGE('',*,*,#5722,.T.);
#7864=ORIENTED_EDGE('',*,*,#5723,.F.);
#7865=ORIENTED_EDGE('',*,*,#5561,.T.);
#7866=ORIENTED_EDGE('',*,*,#5724,.T.);
#7867=ORIENTED_EDGE('',*,*,#5725,.T.);
#7868=ORIENTED_EDGE('',*,*,#5718,.F.);
#7869=ORIENTED_EDGE('',*,*,#5564,.T.);
#7870=ORIENTED_EDGE('',*,*,#5614,.T.);
#7871=ORIENTED_EDGE('',*,*,#5726,.T.);
#7872=ORIENTED_EDGE('',*,*,#5612,.F.);
#7873=ORIENTED_EDGE('',*,*,#5562,.T.);
#7874=ORIENTED_EDGE('',*,*,#5723,.T.);
#7875=ORIENTED_EDGE('',*,*,#5727,.T.);
#7876=ORIENTED_EDGE('',*,*,#5724,.F.);
#7877=ORIENTED_EDGE('',*,*,#5560,.T.);
#7878=ORIENTED_EDGE('',*,*,#5720,.T.);
#7879=ORIENTED_EDGE('',*,*,#5728,.T.);
#7880=ORIENTED_EDGE('',*,*,#5721,.F.);
#7881=ORIENTED_EDGE('',*,*,#5566,.T.);
#7882=ORIENTED_EDGE('',*,*,#5717,.T.);
#7883=ORIENTED_EDGE('',*,*,#5729,.T.);
#7884=ORIENTED_EDGE('',*,*,#5726,.F.);
#7885=ORIENTED_EDGE('',*,*,#5613,.F.);
#7886=ORIENTED_EDGE('',*,*,#5727,.F.);
#7887=ORIENTED_EDGE('',*,*,#5725,.F.);
#7888=ORIENTED_EDGE('',*,*,#5728,.F.);
#7889=ORIENTED_EDGE('',*,*,#5722,.F.);
#7890=ORIENTED_EDGE('',*,*,#5729,.F.);
#7891=ORIENTED_EDGE('',*,*,#5719,.F.);
#7892=ORIENTED_EDGE('',*,*,#5730,.T.);
#7893=ORIENTED_EDGE('',*,*,#5610,.T.);
#7894=ORIENTED_EDGE('',*,*,#5731,.T.);
#7895=ORIENTED_EDGE('',*,*,#5732,.T.);
#7896=ORIENTED_EDGE('',*,*,#5733,.T.);
#7897=ORIENTED_EDGE('',*,*,#5734,.T.);
#7898=ORIENTED_EDGE('',*,*,#5735,.T.);
#7899=ORIENTED_EDGE('',*,*,#5736,.T.);
#7900=ORIENTED_EDGE('',*,*,#5730,.F.);
#7901=ORIENTED_EDGE('',*,*,#5737,.F.);
#7902=ORIENTED_EDGE('',*,*,#5738,.F.);
#7903=ORIENTED_EDGE('',*,*,#5611,.T.);
#7904=ORIENTED_EDGE('',*,*,#5731,.F.);
#7905=ORIENTED_EDGE('',*,*,#5609,.F.);
#7906=ORIENTED_EDGE('',*,*,#5739,.F.);
#7907=ORIENTED_EDGE('',*,*,#5740,.T.);
#7908=ORIENTED_EDGE('',*,*,#5732,.F.);
#7909=ORIENTED_EDGE('',*,*,#5740,.F.);
#7910=ORIENTED_EDGE('',*,*,#5741,.F.);
#7911=ORIENTED_EDGE('',*,*,#5742,.T.);
#7912=ORIENTED_EDGE('',*,*,#5733,.F.);
#7913=ORIENTED_EDGE('',*,*,#5742,.F.);
#7914=ORIENTED_EDGE('',*,*,#5743,.F.);
#7915=ORIENTED_EDGE('',*,*,#5744,.T.);
#7916=ORIENTED_EDGE('',*,*,#5734,.F.);
#7917=ORIENTED_EDGE('',*,*,#5744,.F.);
#7918=ORIENTED_EDGE('',*,*,#5745,.F.);
#7919=ORIENTED_EDGE('',*,*,#5746,.T.);
#7920=ORIENTED_EDGE('',*,*,#5735,.F.);
#7921=ORIENTED_EDGE('',*,*,#5746,.F.);
#7922=ORIENTED_EDGE('',*,*,#5747,.F.);
#7923=ORIENTED_EDGE('',*,*,#5748,.T.);
#7924=ORIENTED_EDGE('',*,*,#5736,.F.);
#7925=ORIENTED_EDGE('',*,*,#5748,.F.);
#7926=ORIENTED_EDGE('',*,*,#5749,.F.);
#7927=ORIENTED_EDGE('',*,*,#5737,.T.);
#7928=ORIENTED_EDGE('',*,*,#5741,.T.);
#7929=ORIENTED_EDGE('',*,*,#5739,.T.);
#7930=ORIENTED_EDGE('',*,*,#5608,.T.);
#7931=ORIENTED_EDGE('',*,*,#5738,.T.);
#7932=ORIENTED_EDGE('',*,*,#5749,.T.);
#7933=ORIENTED_EDGE('',*,*,#5747,.T.);
#7934=ORIENTED_EDGE('',*,*,#5745,.T.);
#7935=ORIENTED_EDGE('',*,*,#5743,.T.);
#7936=ORIENTED_EDGE('',*,*,#5750,.F.);
#7937=ORIENTED_EDGE('',*,*,#5553,.T.);
#7938=ORIENTED_EDGE('',*,*,#5751,.T.);
#7939=ORIENTED_EDGE('',*,*,#5752,.T.);
#7940=ORIENTED_EDGE('',*,*,#5753,.F.);
#7941=ORIENTED_EDGE('',*,*,#5555,.T.);
#7942=ORIENTED_EDGE('',*,*,#5754,.T.);
#7943=ORIENTED_EDGE('',*,*,#5755,.T.);
#7944=ORIENTED_EDGE('',*,*,#5539,.F.);
#7945=ORIENTED_EDGE('',*,*,#5756,.T.);
#7946=ORIENTED_EDGE('',*,*,#5757,.F.);
#7947=ORIENTED_EDGE('',*,*,#5758,.F.);
#7948=ORIENTED_EDGE('',*,*,#5759,.F.);
#7949=ORIENTED_EDGE('',*,*,#5556,.T.);
#7950=ORIENTED_EDGE('',*,*,#5753,.T.);
#7951=ORIENTED_EDGE('',*,*,#5760,.T.);
#7952=ORIENTED_EDGE('',*,*,#5761,.F.);
#7953=ORIENTED_EDGE('',*,*,#5557,.T.);
#7954=ORIENTED_EDGE('',*,*,#5759,.T.);
#7955=ORIENTED_EDGE('',*,*,#5762,.T.);
#7956=ORIENTED_EDGE('',*,*,#5756,.F.);
#7957=ORIENTED_EDGE('',*,*,#5558,.T.);
#7958=ORIENTED_EDGE('',*,*,#5761,.T.);
#7959=ORIENTED_EDGE('',*,*,#5763,.T.);
#7960=ORIENTED_EDGE('',*,*,#5541,.F.);
#7961=ORIENTED_EDGE('',*,*,#5764,.T.);
#7962=ORIENTED_EDGE('',*,*,#5765,.F.);
#7963=ORIENTED_EDGE('',*,*,#5766,.F.);
#7964=ORIENTED_EDGE('',*,*,#5764,.F.);
#7965=ORIENTED_EDGE('',*,*,#5540,.T.);
#7966=ORIENTED_EDGE('',*,*,#5758,.T.);
#7967=ORIENTED_EDGE('',*,*,#5767,.T.);
#7968=ORIENTED_EDGE('',*,*,#5605,.F.);
#7969=ORIENTED_EDGE('',*,*,#5542,.T.);
#7970=ORIENTED_EDGE('',*,*,#5766,.T.);
#7971=ORIENTED_EDGE('',*,*,#5768,.T.);
#7972=ORIENTED_EDGE('',*,*,#5545,.F.);
#7973=ORIENTED_EDGE('',*,*,#5769,.T.);
#7974=ORIENTED_EDGE('',*,*,#5770,.F.);
#7975=ORIENTED_EDGE('',*,*,#5771,.F.);
#7976=ORIENTED_EDGE('',*,*,#5769,.F.);
#7977=ORIENTED_EDGE('',*,*,#5544,.T.);
#7978=ORIENTED_EDGE('',*,*,#5607,.T.);
#7979=ORIENTED_EDGE('',*,*,#5772,.T.);
#7980=ORIENTED_EDGE('',*,*,#5773,.F.);
#7981=ORIENTED_EDGE('',*,*,#5549,.T.);
#7982=ORIENTED_EDGE('',*,*,#5774,.T.);
#7983=ORIENTED_EDGE('',*,*,#5775,.T.);
#7984=ORIENTED_EDGE('',*,*,#5751,.F.);
#7985=ORIENTED_EDGE('',*,*,#5552,.T.);
#7986=ORIENTED_EDGE('',*,*,#5604,.T.);
#7987=ORIENTED_EDGE('',*,*,#5776,.T.);
#7988=ORIENTED_EDGE('',*,*,#5602,.F.);
#7989=ORIENTED_EDGE('',*,*,#5550,.T.);
#7990=ORIENTED_EDGE('',*,*,#5773,.T.);
#7991=ORIENTED_EDGE('',*,*,#5777,.T.);
#7992=ORIENTED_EDGE('',*,*,#5778,.F.);
#7993=ORIENTED_EDGE('',*,*,#5546,.T.);
#7994=ORIENTED_EDGE('',*,*,#5771,.T.);
#7995=ORIENTED_EDGE('',*,*,#5779,.T.);
#7996=ORIENTED_EDGE('',*,*,#5780,.F.);
#7997=ORIENTED_EDGE('',*,*,#5547,.T.);
#7998=ORIENTED_EDGE('',*,*,#5778,.T.);
#7999=ORIENTED_EDGE('',*,*,#5781,.T.);
#8000=ORIENTED_EDGE('',*,*,#5774,.F.);
#8001=ORIENTED_EDGE('',*,*,#5548,.T.);
#8002=ORIENTED_EDGE('',*,*,#5780,.T.);
#8003=ORIENTED_EDGE('',*,*,#5782,.T.);
#8004=ORIENTED_EDGE('',*,*,#5754,.F.);
#8005=ORIENTED_EDGE('',*,*,#5554,.T.);
#8006=ORIENTED_EDGE('',*,*,#5750,.T.);
#8007=ORIENTED_EDGE('',*,*,#5783,.T.);
#8008=ORIENTED_EDGE('',*,*,#5776,.F.);
#8009=ORIENTED_EDGE('',*,*,#5603,.F.);
#8010=ORIENTED_EDGE('',*,*,#5777,.F.);
#8011=ORIENTED_EDGE('',*,*,#5775,.F.);
#8012=ORIENTED_EDGE('',*,*,#5782,.F.);
#8013=ORIENTED_EDGE('',*,*,#5781,.F.);
#8014=ORIENTED_EDGE('',*,*,#5779,.F.);
#8015=ORIENTED_EDGE('',*,*,#5770,.T.);
#8016=ORIENTED_EDGE('',*,*,#5772,.F.);
#8017=ORIENTED_EDGE('',*,*,#5606,.T.);
#8018=ORIENTED_EDGE('',*,*,#5768,.F.);
#8019=ORIENTED_EDGE('',*,*,#5765,.T.);
#8020=ORIENTED_EDGE('',*,*,#5767,.F.);
#8021=ORIENTED_EDGE('',*,*,#5757,.T.);
#8022=ORIENTED_EDGE('',*,*,#5763,.F.);
#8023=ORIENTED_EDGE('',*,*,#5762,.F.);
#8024=ORIENTED_EDGE('',*,*,#5760,.F.);
#8025=ORIENTED_EDGE('',*,*,#5755,.F.);
#8026=ORIENTED_EDGE('',*,*,#5783,.F.);
#8027=ORIENTED_EDGE('',*,*,#5752,.F.);
#8028=ORIENTED_EDGE('',*,*,#5784,.F.);
#8029=ORIENTED_EDGE('',*,*,#5525,.T.);
#8030=ORIENTED_EDGE('',*,*,#5785,.T.);
#8031=ORIENTED_EDGE('',*,*,#5786,.T.);
#8032=ORIENTED_EDGE('',*,*,#5787,.F.);
#8033=ORIENTED_EDGE('',*,*,#5513,.T.);
#8034=ORIENTED_EDGE('',*,*,#5788,.T.);
#8035=ORIENTED_EDGE('',*,*,#5789,.T.);
#8036=ORIENTED_EDGE('',*,*,#5517,.F.);
#8037=ORIENTED_EDGE('',*,*,#5790,.T.);
#8038=ORIENTED_EDGE('',*,*,#5791,.F.);
#8039=ORIENTED_EDGE('',*,*,#5792,.F.);
#8040=ORIENTED_EDGE('',*,*,#5793,.F.);
#8041=ORIENTED_EDGE('',*,*,#5514,.T.);
#8042=ORIENTED_EDGE('',*,*,#5787,.T.);
#8043=ORIENTED_EDGE('',*,*,#5794,.T.);
#8044=ORIENTED_EDGE('',*,*,#5795,.F.);
#8045=ORIENTED_EDGE('',*,*,#5515,.T.);
#8046=ORIENTED_EDGE('',*,*,#5793,.T.);
#8047=ORIENTED_EDGE('',*,*,#5796,.T.);
#8048=ORIENTED_EDGE('',*,*,#5790,.F.);
#8049=ORIENTED_EDGE('',*,*,#5516,.T.);
#8050=ORIENTED_EDGE('',*,*,#5795,.T.);
#8051=ORIENTED_EDGE('',*,*,#5797,.T.);
#8052=ORIENTED_EDGE('',*,*,#5519,.F.);
#8053=ORIENTED_EDGE('',*,*,#5798,.T.);
#8054=ORIENTED_EDGE('',*,*,#5799,.F.);
#8055=ORIENTED_EDGE('',*,*,#5800,.F.);
#8056=ORIENTED_EDGE('',*,*,#5798,.F.);
#8057=ORIENTED_EDGE('',*,*,#5518,.T.);
#8058=ORIENTED_EDGE('',*,*,#5792,.T.);
#8059=ORIENTED_EDGE('',*,*,#5801,.T.);
#8060=ORIENTED_EDGE('',*,*,#5802,.F.);
#8061=ORIENTED_EDGE('',*,*,#5522,.T.);
#8062=ORIENTED_EDGE('',*,*,#5803,.T.);
#8063=ORIENTED_EDGE('',*,*,#5804,.T.);
#8064=ORIENTED_EDGE('',*,*,#5805,.F.);
#8065=ORIENTED_EDGE('',*,*,#5523,.T.);
#8066=ORIENTED_EDGE('',*,*,#5802,.T.);
#8067=ORIENTED_EDGE('',*,*,#5806,.T.);
#8068=ORIENTED_EDGE('',*,*,#5785,.F.);
#8069=ORIENTED_EDGE('',*,*,#5524,.T.);
#8070=ORIENTED_EDGE('',*,*,#5805,.T.);
#8071=ORIENTED_EDGE('',*,*,#5807,.T.);
#8072=ORIENTED_EDGE('',*,*,#5808,.F.);
#8073=ORIENTED_EDGE('',*,*,#5520,.T.);
#8074=ORIENTED_EDGE('',*,*,#5800,.T.);
#8075=ORIENTED_EDGE('',*,*,#5809,.T.);
#8076=ORIENTED_EDGE('',*,*,#5803,.F.);
#8077=ORIENTED_EDGE('',*,*,#5521,.T.);
#8078=ORIENTED_EDGE('',*,*,#5808,.T.);
#8079=ORIENTED_EDGE('',*,*,#5810,.T.);
#8080=ORIENTED_EDGE('',*,*,#5788,.F.);
#8081=ORIENTED_EDGE('',*,*,#5526,.T.);
#8082=ORIENTED_EDGE('',*,*,#5784,.T.);
#8083=ORIENTED_EDGE('',*,*,#5811,.T.);
#8084=ORIENTED_EDGE('',*,*,#5804,.F.);
#8085=ORIENTED_EDGE('',*,*,#5810,.F.);
#8086=ORIENTED_EDGE('',*,*,#5809,.F.);
#8087=ORIENTED_EDGE('',*,*,#5799,.T.);
#8088=ORIENTED_EDGE('',*,*,#5801,.F.);
#8089=ORIENTED_EDGE('',*,*,#5791,.T.);
#8090=ORIENTED_EDGE('',*,*,#5797,.F.);
#8091=ORIENTED_EDGE('',*,*,#5796,.F.);
#8092=ORIENTED_EDGE('',*,*,#5794,.F.);
#8093=ORIENTED_EDGE('',*,*,#5789,.F.);
#8094=ORIENTED_EDGE('',*,*,#5811,.F.);
#8095=ORIENTED_EDGE('',*,*,#5786,.F.);
#8096=ORIENTED_EDGE('',*,*,#5807,.F.);
#8097=ORIENTED_EDGE('',*,*,#5806,.F.);
#8098=ORIENTED_EDGE('',*,*,#5812,.F.);
#8099=ORIENTED_EDGE('',*,*,#5537,.T.);
#8100=ORIENTED_EDGE('',*,*,#5813,.T.);
#8101=ORIENTED_EDGE('',*,*,#5814,.T.);
#8102=ORIENTED_EDGE('',*,*,#5815,.F.);
#8103=ORIENTED_EDGE('',*,*,#5538,.T.);
#8104=ORIENTED_EDGE('',*,*,#5812,.T.);
#8105=ORIENTED_EDGE('',*,*,#5816,.T.);
#8106=ORIENTED_EDGE('',*,*,#5817,.F.);
#8107=ORIENTED_EDGE('',*,*,#5535,.T.);
#8108=ORIENTED_EDGE('',*,*,#5815,.T.);
#8109=ORIENTED_EDGE('',*,*,#5818,.T.);
#8110=ORIENTED_EDGE('',*,*,#5813,.F.);
#8111=ORIENTED_EDGE('',*,*,#5536,.T.);
#8112=ORIENTED_EDGE('',*,*,#5817,.T.);
#8113=ORIENTED_EDGE('',*,*,#5819,.T.);
#8114=ORIENTED_EDGE('',*,*,#5814,.F.);
#8115=ORIENTED_EDGE('',*,*,#5819,.F.);
#8116=ORIENTED_EDGE('',*,*,#5818,.F.);
#8117=ORIENTED_EDGE('',*,*,#5816,.F.);
#8118=ORIENTED_EDGE('',*,*,#5820,.F.);
#8119=ORIENTED_EDGE('',*,*,#5599,.F.);
#8120=ORIENTED_EDGE('',*,*,#5821,.F.);
#8121=ORIENTED_EDGE('',*,*,#5822,.T.);
#8122=ORIENTED_EDGE('',*,*,#5823,.F.);
#8123=ORIENTED_EDGE('',*,*,#5822,.F.);
#8124=ORIENTED_EDGE('',*,*,#5824,.F.);
#8125=ORIENTED_EDGE('',*,*,#5825,.T.);
#8126=ORIENTED_EDGE('',*,*,#5826,.F.);
#8127=ORIENTED_EDGE('',*,*,#5825,.F.);
#8128=ORIENTED_EDGE('',*,*,#5827,.F.);
#8129=ORIENTED_EDGE('',*,*,#5828,.T.);
#8130=ORIENTED_EDGE('',*,*,#5829,.F.);
#8131=ORIENTED_EDGE('',*,*,#5828,.F.);
#8132=ORIENTED_EDGE('',*,*,#5830,.F.);
#8133=ORIENTED_EDGE('',*,*,#5831,.T.);
#8134=ORIENTED_EDGE('',*,*,#5832,.F.);
#8135=ORIENTED_EDGE('',*,*,#5831,.F.);
#8136=ORIENTED_EDGE('',*,*,#5833,.F.);
#8137=ORIENTED_EDGE('',*,*,#5834,.T.);
#8138=ORIENTED_EDGE('',*,*,#5835,.F.);
#8139=ORIENTED_EDGE('',*,*,#5834,.F.);
#8140=ORIENTED_EDGE('',*,*,#5836,.F.);
#8141=ORIENTED_EDGE('',*,*,#5837,.T.);
#8142=ORIENTED_EDGE('',*,*,#5838,.F.);
#8143=ORIENTED_EDGE('',*,*,#5837,.F.);
#8144=ORIENTED_EDGE('',*,*,#5839,.F.);
#8145=ORIENTED_EDGE('',*,*,#5601,.T.);
#8146=ORIENTED_EDGE('',*,*,#5824,.T.);
#8147=ORIENTED_EDGE('',*,*,#5821,.T.);
#8148=ORIENTED_EDGE('',*,*,#5598,.T.);
#8149=ORIENTED_EDGE('',*,*,#5839,.T.);
#8150=ORIENTED_EDGE('',*,*,#5836,.T.);
#8151=ORIENTED_EDGE('',*,*,#5833,.T.);
#8152=ORIENTED_EDGE('',*,*,#5830,.T.);
#8153=ORIENTED_EDGE('',*,*,#5827,.T.);
#8154=ORIENTED_EDGE('',*,*,#5840,.F.);
#8155=ORIENTED_EDGE('',*,*,#5596,.F.);
#8156=ORIENTED_EDGE('',*,*,#5841,.F.);
#8157=ORIENTED_EDGE('',*,*,#5842,.F.);
#8158=ORIENTED_EDGE('',*,*,#5843,.F.);
#8159=ORIENTED_EDGE('',*,*,#5844,.F.);
#8160=ORIENTED_EDGE('',*,*,#5845,.F.);
#8161=ORIENTED_EDGE('',*,*,#5846,.F.);
#8162=ORIENTED_EDGE('',*,*,#5600,.T.);
#8163=ORIENTED_EDGE('',*,*,#5820,.T.);
#8164=ORIENTED_EDGE('',*,*,#5823,.T.);
#8165=ORIENTED_EDGE('',*,*,#5826,.T.);
#8166=ORIENTED_EDGE('',*,*,#5829,.T.);
#8167=ORIENTED_EDGE('',*,*,#5832,.T.);
#8168=ORIENTED_EDGE('',*,*,#5835,.T.);
#8169=ORIENTED_EDGE('',*,*,#5838,.T.);
#8170=ORIENTED_EDGE('',*,*,#5595,.F.);
#8171=ORIENTED_EDGE('',*,*,#5530,.T.);
#8172=ORIENTED_EDGE('',*,*,#5847,.T.);
#8173=ORIENTED_EDGE('',*,*,#5841,.T.);
#8174=ORIENTED_EDGE('',*,*,#5848,.F.);
#8175=ORIENTED_EDGE('',*,*,#5528,.T.);
#8176=ORIENTED_EDGE('',*,*,#5849,.T.);
#8177=ORIENTED_EDGE('',*,*,#5843,.T.);
#8178=ORIENTED_EDGE('',*,*,#5850,.F.);
#8179=ORIENTED_EDGE('',*,*,#5534,.T.);
#8180=ORIENTED_EDGE('',*,*,#5851,.T.);
#8181=ORIENTED_EDGE('',*,*,#5845,.T.);
#8182=ORIENTED_EDGE('',*,*,#5852,.F.);
#8183=ORIENTED_EDGE('',*,*,#5532,.T.);
#8184=ORIENTED_EDGE('',*,*,#5597,.T.);
#8185=ORIENTED_EDGE('',*,*,#5840,.T.);
#8186=ORIENTED_EDGE('',*,*,#5847,.F.);
#8187=ORIENTED_EDGE('',*,*,#5529,.T.);
#8188=ORIENTED_EDGE('',*,*,#5848,.T.);
#8189=ORIENTED_EDGE('',*,*,#5842,.T.);
#8190=ORIENTED_EDGE('',*,*,#5849,.F.);
#8191=ORIENTED_EDGE('',*,*,#5527,.T.);
#8192=ORIENTED_EDGE('',*,*,#5850,.T.);
#8193=ORIENTED_EDGE('',*,*,#5844,.T.);
#8194=ORIENTED_EDGE('',*,*,#5851,.F.);
#8195=ORIENTED_EDGE('',*,*,#5533,.T.);
#8196=ORIENTED_EDGE('',*,*,#5852,.T.);
#8197=ORIENTED_EDGE('',*,*,#5846,.T.);
#8198=ORIENTED_EDGE('',*,*,#5654,.F.);
#8199=ORIENTED_EDGE('',*,*,#5667,.T.);
#8200=ORIENTED_EDGE('',*,*,#5636,.T.);
#8201=ORIENTED_EDGE('',*,*,#5645,.F.);
#8202=ORIENTED_EDGE('',*,*,#5661,.F.);
#8203=ORIENTED_EDGE('',*,*,#5639,.T.);
#8204=ORIENTED_EDGE('',*,*,#5650,.F.);
#8205=ORIENTED_EDGE('',*,*,#5663,.F.);
#8206=ORIENTED_EDGE('',*,*,#5646,.F.);
#8207=ORIENTED_EDGE('',*,*,#5634,.T.);
#8208=ORIENTED_EDGE('',*,*,#5668,.F.);
#8209=ORIENTED_EDGE('',*,*,#5640,.T.);
#8210=ORIENTED_EDGE('',*,*,#5853,.F.);
#8211=ORIENTED_EDGE('',*,*,#5854,.T.);
#8212=ORIENTED_EDGE('',*,*,#5855,.T.);
#8213=ORIENTED_EDGE('',*,*,#5854,.F.);
#8214=ORIENTED_EDGE('',*,*,#5856,.F.);
#8215=ORIENTED_EDGE('',*,*,#5857,.T.);
#8216=ORIENTED_EDGE('',*,*,#5853,.T.);
#8217=ORIENTED_EDGE('',*,*,#5857,.F.);
#8218=ORIENTED_EDGE('',*,*,#5858,.F.);
#8219=ORIENTED_EDGE('',*,*,#5859,.T.);
#8220=ORIENTED_EDGE('',*,*,#5856,.T.);
#8221=ORIENTED_EDGE('',*,*,#5859,.F.);
#8222=ORIENTED_EDGE('',*,*,#5860,.F.);
#8223=ORIENTED_EDGE('',*,*,#5861,.F.);
#8224=ORIENTED_EDGE('',*,*,#5862,.T.);
#8225=ORIENTED_EDGE('',*,*,#5863,.T.);
#8226=ORIENTED_EDGE('',*,*,#5862,.F.);
#8227=ORIENTED_EDGE('',*,*,#5860,.T.);
#8228=ORIENTED_EDGE('',*,*,#5861,.T.);
#8229=ORIENTED_EDGE('',*,*,#5864,.T.);
#8230=ORIENTED_EDGE('',*,*,#5865,.F.);
#8231=ORIENTED_EDGE('',*,*,#5864,.F.);
#8232=ORIENTED_EDGE('',*,*,#5866,.T.);
#8233=ORIENTED_EDGE('',*,*,#5867,.T.);
#8234=ORIENTED_EDGE('',*,*,#5868,.T.);
#8235=ORIENTED_EDGE('',*,*,#5869,.F.);
#8236=ORIENTED_EDGE('',*,*,#5870,.F.);
#8237=ORIENTED_EDGE('',*,*,#5871,.F.);
#8238=ORIENTED_EDGE('',*,*,#5868,.F.);
#8239=ORIENTED_EDGE('',*,*,#5872,.F.);
#8240=ORIENTED_EDGE('',*,*,#5873,.F.);
#8241=ORIENTED_EDGE('',*,*,#5869,.T.);
#8242=ORIENTED_EDGE('',*,*,#5874,.T.);
#8243=ORIENTED_EDGE('',*,*,#5875,.T.);
#8244=ORIENTED_EDGE('',*,*,#5870,.T.);
#8245=ORIENTED_EDGE('',*,*,#5876,.T.);
#8246=ORIENTED_EDGE('',*,*,#5877,.T.);
#8247=ORIENTED_EDGE('',*,*,#5871,.T.);
#8248=ORIENTED_EDGE('',*,*,#5878,.T.);
#8249=ORIENTED_EDGE('',*,*,#5879,.T.);
#8250=ORIENTED_EDGE('',*,*,#5872,.T.);
#8251=ORIENTED_EDGE('',*,*,#5880,.T.);
#8252=ORIENTED_EDGE('',*,*,#5881,.T.);
#8253=ORIENTED_EDGE('',*,*,#5873,.T.);
#8254=ORIENTED_EDGE('',*,*,#5882,.T.);
#8255=ORIENTED_EDGE('',*,*,#5883,.T.);
#8256=ORIENTED_EDGE('',*,*,#5884,.F.);
#8257=ORIENTED_EDGE('',*,*,#5885,.F.);
#8258=ORIENTED_EDGE('',*,*,#5886,.T.);
#8259=ORIENTED_EDGE('',*,*,#5866,.F.);
#8260=ORIENTED_EDGE('',*,*,#5879,.F.);
#8261=ORIENTED_EDGE('',*,*,#5887,.F.);
#8262=ORIENTED_EDGE('',*,*,#5888,.F.);
#8263=ORIENTED_EDGE('',*,*,#5884,.T.);
#8264=ORIENTED_EDGE('',*,*,#5878,.F.);
#8265=ORIENTED_EDGE('',*,*,#5877,.F.);
#8266=ORIENTED_EDGE('',*,*,#5889,.F.);
#8267=ORIENTED_EDGE('',*,*,#5890,.F.);
#8268=ORIENTED_EDGE('',*,*,#5887,.T.);
#8269=ORIENTED_EDGE('',*,*,#5876,.F.);
#8270=ORIENTED_EDGE('',*,*,#5875,.F.);
#8271=ORIENTED_EDGE('',*,*,#5891,.F.);
#8272=ORIENTED_EDGE('',*,*,#5892,.F.);
#8273=ORIENTED_EDGE('',*,*,#5889,.T.);
#8274=ORIENTED_EDGE('',*,*,#5874,.F.);
#8275=ORIENTED_EDGE('',*,*,#5883,.F.);
#8276=ORIENTED_EDGE('',*,*,#5893,.F.);
#8277=ORIENTED_EDGE('',*,*,#5894,.F.);
#8278=ORIENTED_EDGE('',*,*,#5891,.T.);
#8279=ORIENTED_EDGE('',*,*,#5882,.F.);
#8280=ORIENTED_EDGE('',*,*,#5881,.F.);
#8281=ORIENTED_EDGE('',*,*,#5886,.F.);
#8282=ORIENTED_EDGE('',*,*,#5895,.F.);
#8283=ORIENTED_EDGE('',*,*,#5893,.T.);
#8284=ORIENTED_EDGE('',*,*,#5880,.F.);
#8285=ORIENTED_EDGE('',*,*,#5867,.F.);
#8286=ORIENTED_EDGE('',*,*,#5865,.T.);
#8287=ORIENTED_EDGE('',*,*,#5858,.T.);
#8288=ORIENTED_EDGE('',*,*,#5863,.F.);
#8289=ORIENTED_EDGE('',*,*,#5894,.T.);
#8290=ORIENTED_EDGE('',*,*,#5895,.T.);
#8291=ORIENTED_EDGE('',*,*,#5885,.T.);
#8292=ORIENTED_EDGE('',*,*,#5888,.T.);
#8293=ORIENTED_EDGE('',*,*,#5890,.T.);
#8294=ORIENTED_EDGE('',*,*,#5892,.T.);
#8295=ORIENTED_EDGE('',*,*,#5855,.F.);
#8296=ORIENTED_EDGE('',*,*,#5896,.F.);
#8297=ORIENTED_EDGE('',*,*,#5897,.T.);
#8298=ORIENTED_EDGE('',*,*,#5898,.T.);
#8299=ORIENTED_EDGE('',*,*,#5897,.F.);
#8300=ORIENTED_EDGE('',*,*,#5899,.F.);
#8301=ORIENTED_EDGE('',*,*,#5900,.T.);
#8302=ORIENTED_EDGE('',*,*,#5901,.T.);
#8303=ORIENTED_EDGE('',*,*,#5902,.T.);
#8304=ORIENTED_EDGE('',*,*,#5900,.F.);
#8305=ORIENTED_EDGE('',*,*,#5903,.F.);
#8306=ORIENTED_EDGE('',*,*,#5904,.F.);
#8307=ORIENTED_EDGE('',*,*,#5905,.T.);
#8308=ORIENTED_EDGE('',*,*,#5901,.F.);
#8309=ORIENTED_EDGE('',*,*,#5902,.F.);
#8310=ORIENTED_EDGE('',*,*,#5905,.F.);
#8311=ORIENTED_EDGE('',*,*,#5906,.F.);
#8312=ORIENTED_EDGE('',*,*,#5907,.T.);
#8313=ORIENTED_EDGE('',*,*,#5908,.T.);
#8314=ORIENTED_EDGE('',*,*,#5907,.F.);
#8315=ORIENTED_EDGE('',*,*,#5908,.F.);
#8316=ORIENTED_EDGE('',*,*,#5909,.T.);
#8317=ORIENTED_EDGE('',*,*,#5910,.T.);
#8318=ORIENTED_EDGE('',*,*,#5909,.F.);
#8319=ORIENTED_EDGE('',*,*,#5911,.F.);
#8320=ORIENTED_EDGE('',*,*,#5912,.T.);
#8321=ORIENTED_EDGE('',*,*,#5913,.T.);
#8322=ORIENTED_EDGE('',*,*,#5912,.F.);
#8323=ORIENTED_EDGE('',*,*,#5914,.F.);
#8324=ORIENTED_EDGE('',*,*,#5915,.T.);
#8325=ORIENTED_EDGE('',*,*,#5916,.T.);
#8326=ORIENTED_EDGE('',*,*,#5915,.F.);
#8327=ORIENTED_EDGE('',*,*,#5916,.F.);
#8328=ORIENTED_EDGE('',*,*,#5917,.T.);
#8329=ORIENTED_EDGE('',*,*,#5918,.T.);
#8330=ORIENTED_EDGE('',*,*,#5917,.F.);
#8331=ORIENTED_EDGE('',*,*,#5919,.F.);
#8332=ORIENTED_EDGE('',*,*,#5920,.T.);
#8333=ORIENTED_EDGE('',*,*,#5921,.T.);
#8334=ORIENTED_EDGE('',*,*,#5922,.T.);
#8335=ORIENTED_EDGE('',*,*,#5920,.F.);
#8336=ORIENTED_EDGE('',*,*,#5923,.T.);
#8337=ORIENTED_EDGE('',*,*,#5924,.T.);
#8338=ORIENTED_EDGE('',*,*,#5921,.F.);
#8339=ORIENTED_EDGE('',*,*,#5922,.F.);
#8340=ORIENTED_EDGE('',*,*,#5924,.F.);
#8341=ORIENTED_EDGE('',*,*,#5925,.T.);
#8342=ORIENTED_EDGE('',*,*,#5923,.F.);
#8343=ORIENTED_EDGE('',*,*,#5926,.T.);
#8344=ORIENTED_EDGE('',*,*,#5927,.T.);
#8345=ORIENTED_EDGE('',*,*,#5926,.F.);
#8346=ORIENTED_EDGE('',*,*,#5925,.F.);
#8347=ORIENTED_EDGE('',*,*,#5903,.T.);
#8348=ORIENTED_EDGE('',*,*,#5904,.T.);
#8349=ORIENTED_EDGE('',*,*,#5928,.T.);
#8350=ORIENTED_EDGE('',*,*,#5906,.T.);
#8351=ORIENTED_EDGE('',*,*,#5928,.F.);
#8352=ORIENTED_EDGE('',*,*,#5918,.F.);
#8353=ORIENTED_EDGE('',*,*,#5919,.T.);
#8354=ORIENTED_EDGE('',*,*,#5913,.F.);
#8355=ORIENTED_EDGE('',*,*,#5914,.T.);
#8356=ORIENTED_EDGE('',*,*,#5911,.T.);
#8357=ORIENTED_EDGE('',*,*,#5910,.F.);
#8358=ORIENTED_EDGE('',*,*,#5899,.T.);
#8359=ORIENTED_EDGE('',*,*,#5898,.F.);
#8360=ORIENTED_EDGE('',*,*,#5927,.F.);
#8361=ORIENTED_EDGE('',*,*,#5896,.T.);
#8362=ORIENTED_EDGE('',*,*,#5929,.F.);
#8363=ORIENTED_EDGE('',*,*,#5930,.T.);
#8364=ORIENTED_EDGE('',*,*,#5931,.T.);
#8365=ORIENTED_EDGE('',*,*,#5932,.T.);
#8366=ORIENTED_EDGE('',*,*,#5933,.T.);
#8367=ORIENTED_EDGE('',*,*,#5934,.T.);
#8368=ORIENTED_EDGE('',*,*,#5935,.T.);
#8369=ORIENTED_EDGE('',*,*,#5936,.T.);
#8370=ORIENTED_EDGE('',*,*,#5930,.F.);
#8371=ORIENTED_EDGE('',*,*,#5937,.T.);
#8372=ORIENTED_EDGE('',*,*,#5938,.T.);
#8373=ORIENTED_EDGE('',*,*,#5939,.F.);
#8374=ORIENTED_EDGE('',*,*,#5938,.F.);
#8375=ORIENTED_EDGE('',*,*,#5940,.T.);
#8376=ORIENTED_EDGE('',*,*,#5937,.F.);
#8377=ORIENTED_EDGE('',*,*,#5941,.T.);
#8378=ORIENTED_EDGE('',*,*,#5942,.T.);
#8379=ORIENTED_EDGE('',*,*,#5941,.F.);
#8380=ORIENTED_EDGE('',*,*,#5940,.F.);
#8381=ORIENTED_EDGE('',*,*,#5942,.F.);
#8382=ORIENTED_EDGE('',*,*,#5943,.T.);
#8383=ORIENTED_EDGE('',*,*,#5944,.T.);
#8384=ORIENTED_EDGE('',*,*,#5943,.F.);
#8385=ORIENTED_EDGE('',*,*,#5945,.T.);
#8386=ORIENTED_EDGE('',*,*,#5946,.T.);
#8387=ORIENTED_EDGE('',*,*,#5947,.T.);
#8388=ORIENTED_EDGE('',*,*,#5948,.F.);
#8389=ORIENTED_EDGE('',*,*,#5949,.F.);
#8390=ORIENTED_EDGE('',*,*,#5950,.F.);
#8391=ORIENTED_EDGE('',*,*,#5947,.F.);
#8392=ORIENTED_EDGE('',*,*,#5951,.F.);
#8393=ORIENTED_EDGE('',*,*,#5952,.F.);
#8394=ORIENTED_EDGE('',*,*,#5939,.T.);
#8395=ORIENTED_EDGE('',*,*,#5948,.T.);
#8396=ORIENTED_EDGE('',*,*,#5953,.T.);
#8397=ORIENTED_EDGE('',*,*,#5954,.T.);
#8398=ORIENTED_EDGE('',*,*,#5949,.T.);
#8399=ORIENTED_EDGE('',*,*,#5955,.T.);
#8400=ORIENTED_EDGE('',*,*,#5956,.T.);
#8401=ORIENTED_EDGE('',*,*,#5950,.T.);
#8402=ORIENTED_EDGE('',*,*,#5957,.T.);
#8403=ORIENTED_EDGE('',*,*,#5958,.T.);
#8404=ORIENTED_EDGE('',*,*,#5951,.T.);
#8405=ORIENTED_EDGE('',*,*,#5959,.T.);
#8406=ORIENTED_EDGE('',*,*,#5960,.T.);
#8407=ORIENTED_EDGE('',*,*,#5952,.T.);
#8408=ORIENTED_EDGE('',*,*,#5961,.T.);
#8409=ORIENTED_EDGE('',*,*,#5962,.T.);
#8410=ORIENTED_EDGE('',*,*,#5963,.F.);
#8411=ORIENTED_EDGE('',*,*,#5964,.F.);
#8412=ORIENTED_EDGE('',*,*,#5965,.F.);
#8413=ORIENTED_EDGE('',*,*,#5966,.T.);
#8414=ORIENTED_EDGE('',*,*,#5945,.F.);
#8415=ORIENTED_EDGE('',*,*,#5958,.F.);
#8416=ORIENTED_EDGE('',*,*,#5967,.F.);
#8417=ORIENTED_EDGE('',*,*,#5968,.F.);
#8418=ORIENTED_EDGE('',*,*,#5969,.F.);
#8419=ORIENTED_EDGE('',*,*,#5963,.T.);
#8420=ORIENTED_EDGE('',*,*,#5957,.F.);
#8421=ORIENTED_EDGE('',*,*,#5956,.F.);
#8422=ORIENTED_EDGE('',*,*,#5970,.F.);
#8423=ORIENTED_EDGE('',*,*,#5971,.F.);
#8424=ORIENTED_EDGE('',*,*,#5972,.F.);
#8425=ORIENTED_EDGE('',*,*,#5967,.T.);
#8426=ORIENTED_EDGE('',*,*,#5955,.F.);
#8427=ORIENTED_EDGE('',*,*,#5954,.F.);
#8428=ORIENTED_EDGE('',*,*,#5973,.F.);
#8429=ORIENTED_EDGE('',*,*,#5974,.F.);
#8430=ORIENTED_EDGE('',*,*,#5975,.F.);
#8431=ORIENTED_EDGE('',*,*,#5970,.T.);
#8432=ORIENTED_EDGE('',*,*,#5953,.F.);
#8433=ORIENTED_EDGE('',*,*,#5962,.F.);
#8434=ORIENTED_EDGE('',*,*,#5976,.F.);
#8435=ORIENTED_EDGE('',*,*,#5977,.F.);
#8436=ORIENTED_EDGE('',*,*,#5978,.F.);
#8437=ORIENTED_EDGE('',*,*,#5973,.T.);
#8438=ORIENTED_EDGE('',*,*,#5961,.F.);
#8439=ORIENTED_EDGE('',*,*,#5960,.F.);
#8440=ORIENTED_EDGE('',*,*,#5966,.F.);
#8441=ORIENTED_EDGE('',*,*,#5979,.F.);
#8442=ORIENTED_EDGE('',*,*,#5980,.F.);
#8443=ORIENTED_EDGE('',*,*,#5976,.T.);
#8444=ORIENTED_EDGE('',*,*,#5959,.F.);
#8445=ORIENTED_EDGE('',*,*,#5946,.F.);
#8446=ORIENTED_EDGE('',*,*,#5929,.T.);
#8447=ORIENTED_EDGE('',*,*,#5944,.F.);
#8448=ORIENTED_EDGE('',*,*,#5964,.T.);
#8449=ORIENTED_EDGE('',*,*,#5969,.T.);
#8450=ORIENTED_EDGE('',*,*,#5932,.F.);
#8451=ORIENTED_EDGE('',*,*,#5931,.F.);
#8452=ORIENTED_EDGE('',*,*,#5979,.T.);
#8453=ORIENTED_EDGE('',*,*,#5965,.T.);
#8454=ORIENTED_EDGE('',*,*,#5968,.T.);
#8455=ORIENTED_EDGE('',*,*,#5972,.T.);
#8456=ORIENTED_EDGE('',*,*,#5933,.F.);
#8457=ORIENTED_EDGE('',*,*,#5936,.F.);
#8458=ORIENTED_EDGE('',*,*,#5977,.T.);
#8459=ORIENTED_EDGE('',*,*,#5980,.T.);
#8460=ORIENTED_EDGE('',*,*,#5935,.F.);
#8461=ORIENTED_EDGE('',*,*,#5974,.T.);
#8462=ORIENTED_EDGE('',*,*,#5978,.T.);
#8463=ORIENTED_EDGE('',*,*,#5971,.T.);
#8464=ORIENTED_EDGE('',*,*,#5975,.T.);
#8465=ORIENTED_EDGE('',*,*,#5934,.F.);
#8466=ORIENTED_EDGE('',*,*,#5981,.F.);
#8467=ORIENTED_EDGE('',*,*,#5982,.F.);
#8468=ORIENTED_EDGE('',*,*,#5983,.F.);
#8469=ORIENTED_EDGE('',*,*,#5984,.T.);
#8470=ORIENTED_EDGE('',*,*,#5985,.F.);
#8471=ORIENTED_EDGE('',*,*,#5986,.F.);
#8472=ORIENTED_EDGE('',*,*,#5987,.T.);
#8473=ORIENTED_EDGE('',*,*,#5982,.T.);
#8474=ORIENTED_EDGE('',*,*,#5988,.T.);
#8475=ORIENTED_EDGE('',*,*,#5989,.T.);
#8476=ORIENTED_EDGE('',*,*,#5990,.F.);
#8477=ORIENTED_EDGE('',*,*,#5983,.T.);
#8478=ORIENTED_EDGE('',*,*,#5987,.F.);
#8479=ORIENTED_EDGE('',*,*,#5991,.F.);
#8480=ORIENTED_EDGE('',*,*,#5992,.T.);
#8481=ORIENTED_EDGE('',*,*,#5993,.T.);
#8482=ORIENTED_EDGE('',*,*,#5992,.F.);
#8483=ORIENTED_EDGE('',*,*,#5994,.F.);
#8484=ORIENTED_EDGE('',*,*,#5995,.T.);
#8485=ORIENTED_EDGE('',*,*,#5991,.T.);
#8486=ORIENTED_EDGE('',*,*,#5995,.F.);
#8487=ORIENTED_EDGE('',*,*,#5996,.F.);
#8488=ORIENTED_EDGE('',*,*,#5997,.T.);
#8489=ORIENTED_EDGE('',*,*,#5998,.T.);
#8490=ORIENTED_EDGE('',*,*,#5997,.F.);
#8491=ORIENTED_EDGE('',*,*,#5999,.F.);
#8492=ORIENTED_EDGE('',*,*,#6000,.T.);
#8493=ORIENTED_EDGE('',*,*,#5996,.T.);
#8494=ORIENTED_EDGE('',*,*,#6000,.F.);
#8495=ORIENTED_EDGE('',*,*,#6001,.F.);
#8496=ORIENTED_EDGE('',*,*,#6002,.T.);
#8497=ORIENTED_EDGE('',*,*,#5986,.T.);
#8498=ORIENTED_EDGE('',*,*,#6002,.F.);
#8499=ORIENTED_EDGE('',*,*,#6003,.F.);
#8500=ORIENTED_EDGE('',*,*,#6004,.T.);
#8501=ORIENTED_EDGE('',*,*,#6001,.T.);
#8502=ORIENTED_EDGE('',*,*,#6004,.F.);
#8503=ORIENTED_EDGE('',*,*,#6005,.F.);
#8504=ORIENTED_EDGE('',*,*,#6006,.F.);
#8505=ORIENTED_EDGE('',*,*,#6007,.T.);
#8506=ORIENTED_EDGE('',*,*,#6008,.T.);
#8507=ORIENTED_EDGE('',*,*,#6007,.F.);
#8508=ORIENTED_EDGE('',*,*,#6005,.T.);
#8509=ORIENTED_EDGE('',*,*,#6006,.T.);
#8510=ORIENTED_EDGE('',*,*,#6009,.T.);
#8511=ORIENTED_EDGE('',*,*,#6010,.F.);
#8512=ORIENTED_EDGE('',*,*,#6009,.F.);
#8513=ORIENTED_EDGE('',*,*,#6011,.F.);
#8514=ORIENTED_EDGE('',*,*,#6012,.T.);
#8515=ORIENTED_EDGE('',*,*,#6013,.T.);
#8516=ORIENTED_EDGE('',*,*,#6012,.F.);
#8517=ORIENTED_EDGE('',*,*,#6014,.F.);
#8518=ORIENTED_EDGE('',*,*,#6015,.T.);
#8519=ORIENTED_EDGE('',*,*,#6011,.T.);
#8520=ORIENTED_EDGE('',*,*,#6015,.F.);
#8521=ORIENTED_EDGE('',*,*,#6016,.F.);
#8522=ORIENTED_EDGE('',*,*,#6017,.T.);
#8523=ORIENTED_EDGE('',*,*,#6014,.T.);
#8524=ORIENTED_EDGE('',*,*,#6017,.F.);
#8525=ORIENTED_EDGE('',*,*,#6018,.F.);
#8526=ORIENTED_EDGE('',*,*,#5988,.F.);
#8527=ORIENTED_EDGE('',*,*,#5981,.T.);
#8528=ORIENTED_EDGE('',*,*,#5990,.T.);
#8529=ORIENTED_EDGE('',*,*,#6019,.T.);
#8530=ORIENTED_EDGE('',*,*,#5984,.F.);
#8531=ORIENTED_EDGE('',*,*,#6016,.T.);
#8532=ORIENTED_EDGE('',*,*,#6010,.T.);
#8533=ORIENTED_EDGE('',*,*,#6013,.F.);
#8534=ORIENTED_EDGE('',*,*,#6008,.F.);
#8535=ORIENTED_EDGE('',*,*,#6003,.T.);
#8536=ORIENTED_EDGE('',*,*,#5994,.T.);
#8537=ORIENTED_EDGE('',*,*,#5998,.F.);
#8538=ORIENTED_EDGE('',*,*,#5993,.F.);
#8539=ORIENTED_EDGE('',*,*,#6019,.F.);
#8540=ORIENTED_EDGE('',*,*,#5989,.F.);
#8541=ORIENTED_EDGE('',*,*,#6018,.T.);
#8542=ORIENTED_EDGE('',*,*,#5985,.T.);
#8543=ORIENTED_EDGE('',*,*,#5999,.T.);
#8544=ORIENTED_EDGE('',*,*,#6020,.F.);
#8545=ORIENTED_EDGE('',*,*,#6021,.T.);
#8546=ORIENTED_EDGE('',*,*,#6022,.F.);
#8547=ORIENTED_EDGE('',*,*,#6021,.F.);
#8548=ORIENTED_EDGE('',*,*,#6023,.F.);
#8549=ORIENTED_EDGE('',*,*,#6024,.F.);
#8550=ORIENTED_EDGE('',*,*,#6025,.T.);
#8551=ORIENTED_EDGE('',*,*,#6020,.T.);
#8552=ORIENTED_EDGE('',*,*,#6025,.F.);
#8553=ORIENTED_EDGE('',*,*,#6026,.F.);
#8554=ORIENTED_EDGE('',*,*,#6027,.T.);
#8555=ORIENTED_EDGE('',*,*,#6028,.T.);
#8556=ORIENTED_EDGE('',*,*,#6027,.F.);
#8557=ORIENTED_EDGE('',*,*,#6029,.F.);
#8558=ORIENTED_EDGE('',*,*,#6030,.T.);
#8559=ORIENTED_EDGE('',*,*,#6031,.T.);
#8560=ORIENTED_EDGE('',*,*,#6032,.T.);
#8561=ORIENTED_EDGE('',*,*,#6030,.F.);
#8562=ORIENTED_EDGE('',*,*,#6023,.T.);
#8563=ORIENTED_EDGE('',*,*,#6024,.T.);
#8564=ORIENTED_EDGE('',*,*,#6033,.T.);
#8565=ORIENTED_EDGE('',*,*,#6031,.F.);
#8566=ORIENTED_EDGE('',*,*,#6032,.F.);
#8567=ORIENTED_EDGE('',*,*,#6033,.F.);
#8568=ORIENTED_EDGE('',*,*,#6022,.T.);
#8569=ORIENTED_EDGE('',*,*,#6034,.T.);
#8570=ORIENTED_EDGE('',*,*,#6035,.T.);
#8571=ORIENTED_EDGE('',*,*,#6034,.F.);
#8572=ORIENTED_EDGE('',*,*,#6035,.F.);
#8573=ORIENTED_EDGE('',*,*,#6036,.T.);
#8574=ORIENTED_EDGE('',*,*,#6037,.T.);
#8575=ORIENTED_EDGE('',*,*,#6036,.F.);
#8576=ORIENTED_EDGE('',*,*,#6038,.F.);
#8577=ORIENTED_EDGE('',*,*,#6039,.T.);
#8578=ORIENTED_EDGE('',*,*,#6040,.T.);
#8579=ORIENTED_EDGE('',*,*,#6039,.F.);
#8580=ORIENTED_EDGE('',*,*,#6040,.F.);
#8581=ORIENTED_EDGE('',*,*,#6041,.T.);
#8582=ORIENTED_EDGE('',*,*,#6042,.T.);
#8583=ORIENTED_EDGE('',*,*,#6043,.T.);
#8584=ORIENTED_EDGE('',*,*,#6041,.F.);
#8585=ORIENTED_EDGE('',*,*,#6044,.T.);
#8586=ORIENTED_EDGE('',*,*,#6045,.T.);
#8587=ORIENTED_EDGE('',*,*,#6042,.F.);
#8588=ORIENTED_EDGE('',*,*,#6043,.F.);
#8589=ORIENTED_EDGE('',*,*,#6045,.F.);
#8590=ORIENTED_EDGE('',*,*,#6046,.T.);
#8591=ORIENTED_EDGE('',*,*,#6044,.F.);
#8592=ORIENTED_EDGE('',*,*,#6047,.T.);
#8593=ORIENTED_EDGE('',*,*,#6048,.T.);
#8594=ORIENTED_EDGE('',*,*,#6047,.F.);
#8595=ORIENTED_EDGE('',*,*,#6046,.F.);
#8596=ORIENTED_EDGE('',*,*,#6049,.T.);
#8597=ORIENTED_EDGE('',*,*,#6050,.F.);
#8598=ORIENTED_EDGE('',*,*,#6051,.T.);
#8599=ORIENTED_EDGE('',*,*,#6052,.T.);
#8600=ORIENTED_EDGE('',*,*,#6053,.T.);
#8601=ORIENTED_EDGE('',*,*,#6054,.F.);
#8602=ORIENTED_EDGE('',*,*,#6055,.T.);
#8603=ORIENTED_EDGE('',*,*,#6050,.T.);
#8604=ORIENTED_EDGE('',*,*,#6056,.T.);
#8605=ORIENTED_EDGE('',*,*,#6057,.F.);
#8606=ORIENTED_EDGE('',*,*,#6058,.T.);
#8607=ORIENTED_EDGE('',*,*,#6054,.T.);
#8608=ORIENTED_EDGE('',*,*,#6059,.T.);
#8609=ORIENTED_EDGE('',*,*,#6060,.F.);
#8610=ORIENTED_EDGE('',*,*,#6061,.T.);
#8611=ORIENTED_EDGE('',*,*,#6057,.T.);
#8612=ORIENTED_EDGE('',*,*,#6062,.T.);
#8613=ORIENTED_EDGE('',*,*,#6063,.F.);
#8614=ORIENTED_EDGE('',*,*,#6064,.T.);
#8615=ORIENTED_EDGE('',*,*,#6060,.T.);
#8616=ORIENTED_EDGE('',*,*,#6065,.T.);
#8617=ORIENTED_EDGE('',*,*,#6066,.F.);
#8618=ORIENTED_EDGE('',*,*,#6067,.T.);
#8619=ORIENTED_EDGE('',*,*,#6063,.T.);
#8620=ORIENTED_EDGE('',*,*,#6068,.T.);
#8621=ORIENTED_EDGE('',*,*,#6069,.F.);
#8622=ORIENTED_EDGE('',*,*,#6070,.T.);
#8623=ORIENTED_EDGE('',*,*,#6066,.T.);
#8624=ORIENTED_EDGE('',*,*,#6071,.T.);
#8625=ORIENTED_EDGE('',*,*,#6052,.F.);
#8626=ORIENTED_EDGE('',*,*,#6072,.T.);
#8627=ORIENTED_EDGE('',*,*,#6069,.T.);
#8628=ORIENTED_EDGE('',*,*,#6072,.F.);
#8629=ORIENTED_EDGE('',*,*,#6051,.F.);
#8630=ORIENTED_EDGE('',*,*,#6055,.F.);
#8631=ORIENTED_EDGE('',*,*,#6058,.F.);
#8632=ORIENTED_EDGE('',*,*,#6061,.F.);
#8633=ORIENTED_EDGE('',*,*,#6064,.F.);
#8634=ORIENTED_EDGE('',*,*,#6067,.F.);
#8635=ORIENTED_EDGE('',*,*,#6070,.F.);
#8636=ORIENTED_EDGE('',*,*,#6038,.T.);
#8637=ORIENTED_EDGE('',*,*,#6071,.F.);
#8638=ORIENTED_EDGE('',*,*,#6068,.F.);
#8639=ORIENTED_EDGE('',*,*,#6065,.F.);
#8640=ORIENTED_EDGE('',*,*,#6062,.F.);
#8641=ORIENTED_EDGE('',*,*,#6059,.F.);
#8642=ORIENTED_EDGE('',*,*,#6056,.F.);
#8643=ORIENTED_EDGE('',*,*,#6053,.F.);
#8644=ORIENTED_EDGE('',*,*,#6049,.F.);
#8645=ORIENTED_EDGE('',*,*,#6037,.F.);
#8646=ORIENTED_EDGE('',*,*,#6029,.T.);
#8647=ORIENTED_EDGE('',*,*,#6028,.F.);
#8648=ORIENTED_EDGE('',*,*,#6048,.F.);
#8649=ORIENTED_EDGE('',*,*,#6026,.T.);
#8650=ORIENTED_EDGE('',*,*,#6073,.F.);
#8651=ORIENTED_EDGE('',*,*,#6074,.T.);
#8652=ORIENTED_EDGE('',*,*,#6075,.T.);
#8653=ORIENTED_EDGE('',*,*,#6074,.F.);
#8654=ORIENTED_EDGE('',*,*,#6076,.T.);
#8655=ORIENTED_EDGE('',*,*,#6077,.T.);
#8656=ORIENTED_EDGE('',*,*,#6078,.F.);
#8657=ORIENTED_EDGE('',*,*,#6077,.F.);
#8658=ORIENTED_EDGE('',*,*,#6079,.F.);
#8659=ORIENTED_EDGE('',*,*,#6080,.T.);
#8660=ORIENTED_EDGE('',*,*,#6081,.T.);
#8661=ORIENTED_EDGE('',*,*,#6080,.F.);
#8662=ORIENTED_EDGE('',*,*,#6082,.F.);
#8663=ORIENTED_EDGE('',*,*,#6083,.T.);
#8664=ORIENTED_EDGE('',*,*,#6084,.T.);
#8665=ORIENTED_EDGE('',*,*,#6083,.F.);
#8666=ORIENTED_EDGE('',*,*,#6085,.F.);
#8667=ORIENTED_EDGE('',*,*,#6086,.T.);
#8668=ORIENTED_EDGE('',*,*,#6082,.T.);
#8669=ORIENTED_EDGE('',*,*,#6086,.F.);
#8670=ORIENTED_EDGE('',*,*,#6087,.F.);
#8671=ORIENTED_EDGE('',*,*,#6088,.T.);
#8672=ORIENTED_EDGE('',*,*,#6085,.T.);
#8673=ORIENTED_EDGE('',*,*,#6088,.F.);
#8674=ORIENTED_EDGE('',*,*,#6089,.F.);
#8675=ORIENTED_EDGE('',*,*,#6090,.T.);
#8676=ORIENTED_EDGE('',*,*,#6091,.T.);
#8677=ORIENTED_EDGE('',*,*,#6090,.F.);
#8678=ORIENTED_EDGE('',*,*,#6092,.F.);
#8679=ORIENTED_EDGE('',*,*,#6093,.T.);
#8680=ORIENTED_EDGE('',*,*,#6094,.T.);
#8681=ORIENTED_EDGE('',*,*,#6093,.F.);
#8682=ORIENTED_EDGE('',*,*,#6095,.T.);
#8683=ORIENTED_EDGE('',*,*,#6096,.T.);
#8684=ORIENTED_EDGE('',*,*,#6097,.F.);
#8685=ORIENTED_EDGE('',*,*,#6096,.F.);
#8686=ORIENTED_EDGE('',*,*,#6098,.F.);
#8687=ORIENTED_EDGE('',*,*,#6099,.T.);
#8688=ORIENTED_EDGE('',*,*,#6100,.T.);
#8689=ORIENTED_EDGE('',*,*,#6099,.F.);
#8690=ORIENTED_EDGE('',*,*,#6097,.T.);
#8691=ORIENTED_EDGE('',*,*,#6100,.F.);
#8692=ORIENTED_EDGE('',*,*,#6092,.T.);
#8693=ORIENTED_EDGE('',*,*,#6095,.F.);
#8694=ORIENTED_EDGE('',*,*,#6089,.T.);
#8695=ORIENTED_EDGE('',*,*,#6094,.F.);
#8696=ORIENTED_EDGE('',*,*,#6087,.T.);
#8697=ORIENTED_EDGE('',*,*,#6091,.F.);
#8698=ORIENTED_EDGE('',*,*,#6084,.F.);
#8699=ORIENTED_EDGE('',*,*,#6079,.T.);
#8700=ORIENTED_EDGE('',*,*,#6081,.F.);
#8701=ORIENTED_EDGE('',*,*,#6078,.T.);
#8702=ORIENTED_EDGE('',*,*,#6076,.F.);
#8703=ORIENTED_EDGE('',*,*,#6073,.T.);
#8704=ORIENTED_EDGE('',*,*,#6075,.F.);
#8705=ORIENTED_EDGE('',*,*,#6098,.T.);
#8706=ORIENTED_EDGE('',*,*,#6101,.F.);
#8707=ORIENTED_EDGE('',*,*,#6102,.T.);
#8708=ORIENTED_EDGE('',*,*,#6103,.T.);
#8709=ORIENTED_EDGE('',*,*,#6102,.F.);
#8710=ORIENTED_EDGE('',*,*,#6104,.F.);
#8711=ORIENTED_EDGE('',*,*,#6105,.T.);
#8712=ORIENTED_EDGE('',*,*,#6106,.T.);
#8713=ORIENTED_EDGE('',*,*,#6105,.F.);
#8714=ORIENTED_EDGE('',*,*,#6106,.F.);
#8715=ORIENTED_EDGE('',*,*,#6107,.T.);
#8716=ORIENTED_EDGE('',*,*,#6108,.T.);
#8717=ORIENTED_EDGE('',*,*,#6107,.F.);
#8718=ORIENTED_EDGE('',*,*,#6108,.F.);
#8719=ORIENTED_EDGE('',*,*,#6109,.T.);
#8720=ORIENTED_EDGE('',*,*,#6110,.T.);
#8721=ORIENTED_EDGE('',*,*,#6109,.F.);
#8722=ORIENTED_EDGE('',*,*,#6111,.F.);
#8723=ORIENTED_EDGE('',*,*,#6112,.T.);
#8724=ORIENTED_EDGE('',*,*,#6113,.T.);
#8725=ORIENTED_EDGE('',*,*,#6112,.F.);
#8726=ORIENTED_EDGE('',*,*,#6114,.F.);
#8727=ORIENTED_EDGE('',*,*,#6115,.T.);
#8728=ORIENTED_EDGE('',*,*,#6116,.T.);
#8729=ORIENTED_EDGE('',*,*,#6117,.T.);
#8730=ORIENTED_EDGE('',*,*,#6115,.F.);
#8731=ORIENTED_EDGE('',*,*,#6118,.T.);
#8732=ORIENTED_EDGE('',*,*,#6119,.T.);
#8733=ORIENTED_EDGE('',*,*,#6116,.F.);
#8734=ORIENTED_EDGE('',*,*,#6117,.F.);
#8735=ORIENTED_EDGE('',*,*,#6119,.F.);
#8736=ORIENTED_EDGE('',*,*,#6120,.T.);
#8737=ORIENTED_EDGE('',*,*,#6118,.F.);
#8738=ORIENTED_EDGE('',*,*,#6121,.T.);
#8739=ORIENTED_EDGE('',*,*,#6122,.T.);
#8740=ORIENTED_EDGE('',*,*,#6123,.T.);
#8741=ORIENTED_EDGE('',*,*,#6121,.F.);
#8742=ORIENTED_EDGE('',*,*,#6120,.F.);
#8743=ORIENTED_EDGE('',*,*,#6124,.T.);
#8744=ORIENTED_EDGE('',*,*,#6125,.T.);
#8745=ORIENTED_EDGE('',*,*,#6122,.F.);
#8746=ORIENTED_EDGE('',*,*,#6123,.F.);
#8747=ORIENTED_EDGE('',*,*,#6125,.F.);
#8748=ORIENTED_EDGE('',*,*,#6126,.T.);
#8749=ORIENTED_EDGE('',*,*,#6124,.F.);
#8750=ORIENTED_EDGE('',*,*,#6127,.T.);
#8751=ORIENTED_EDGE('',*,*,#6128,.T.);
#8752=ORIENTED_EDGE('',*,*,#6127,.F.);
#8753=ORIENTED_EDGE('',*,*,#6126,.F.);
#8754=ORIENTED_EDGE('',*,*,#6128,.F.);
#8755=ORIENTED_EDGE('',*,*,#6129,.T.);
#8756=ORIENTED_EDGE('',*,*,#6130,.T.);
#8757=ORIENTED_EDGE('',*,*,#6129,.F.);
#8758=ORIENTED_EDGE('',*,*,#6130,.F.);
#8759=ORIENTED_EDGE('',*,*,#6131,.T.);
#8760=ORIENTED_EDGE('',*,*,#6132,.T.);
#8761=ORIENTED_EDGE('',*,*,#6131,.F.);
#8762=ORIENTED_EDGE('',*,*,#6132,.F.);
#8763=ORIENTED_EDGE('',*,*,#6133,.T.);
#8764=ORIENTED_EDGE('',*,*,#6134,.T.);
#8765=ORIENTED_EDGE('',*,*,#6133,.F.);
#8766=ORIENTED_EDGE('',*,*,#6114,.T.);
#8767=ORIENTED_EDGE('',*,*,#6113,.F.);
#8768=ORIENTED_EDGE('',*,*,#6110,.F.);
#8769=ORIENTED_EDGE('',*,*,#6111,.T.);
#8770=ORIENTED_EDGE('',*,*,#6104,.T.);
#8771=ORIENTED_EDGE('',*,*,#6103,.F.);
#8772=ORIENTED_EDGE('',*,*,#6134,.F.);
#8773=ORIENTED_EDGE('',*,*,#6101,.T.);
#8774=ORIENTED_EDGE('',*,*,#6135,.F.);
#8775=ORIENTED_EDGE('',*,*,#6136,.T.);
#8776=ORIENTED_EDGE('',*,*,#6137,.T.);
#8777=ORIENTED_EDGE('',*,*,#6136,.F.);
#8778=ORIENTED_EDGE('',*,*,#6138,.F.);
#8779=ORIENTED_EDGE('',*,*,#6139,.T.);
#8780=ORIENTED_EDGE('',*,*,#6140,.T.);
#8781=ORIENTED_EDGE('',*,*,#6139,.F.);
#8782=ORIENTED_EDGE('',*,*,#6138,.T.);
#8783=ORIENTED_EDGE('',*,*,#6137,.F.);
#8784=ORIENTED_EDGE('',*,*,#6140,.F.);
#8785=ORIENTED_EDGE('',*,*,#6135,.T.);
#8786=ORIENTED_EDGE('',*,*,#6141,.T.);
#8787=ORIENTED_EDGE('',*,*,#6142,.T.);
#8788=ORIENTED_EDGE('',*,*,#6143,.F.);
#8789=ORIENTED_EDGE('',*,*,#6142,.F.);
#8790=ORIENTED_EDGE('',*,*,#6144,.T.);
#8791=ORIENTED_EDGE('',*,*,#6141,.F.);
#8792=ORIENTED_EDGE('',*,*,#6145,.T.);
#8793=ORIENTED_EDGE('',*,*,#6146,.T.);
#8794=ORIENTED_EDGE('',*,*,#6145,.F.);
#8795=ORIENTED_EDGE('',*,*,#6144,.F.);
#8796=ORIENTED_EDGE('',*,*,#6146,.F.);
#8797=ORIENTED_EDGE('',*,*,#6147,.T.);
#8798=ORIENTED_EDGE('',*,*,#6148,.T.);
#8799=ORIENTED_EDGE('',*,*,#6147,.F.);
#8800=ORIENTED_EDGE('',*,*,#6149,.F.);
#8801=ORIENTED_EDGE('',*,*,#6150,.T.);
#8802=ORIENTED_EDGE('',*,*,#6151,.T.);
#8803=ORIENTED_EDGE('',*,*,#6150,.F.);
#8804=ORIENTED_EDGE('',*,*,#6149,.T.);
#8805=ORIENTED_EDGE('',*,*,#6148,.F.);
#8806=ORIENTED_EDGE('',*,*,#6151,.F.);
#8807=ORIENTED_EDGE('',*,*,#6143,.T.);
#8808=CYLINDRICAL_SURFACE('',#9751,6.00000000000002);
#8809=CYLINDRICAL_SURFACE('',#9754,6.00000000000001);
#8810=CYLINDRICAL_SURFACE('',#9757,6.00000000000002);
#8811=CYLINDRICAL_SURFACE('',#9760,6.00000000000001);
#8812=CYLINDRICAL_SURFACE('',#9763,6.34999999999999);
#8813=CYLINDRICAL_SURFACE('',#9766,6.35000000000122);
#8814=CYLINDRICAL_SURFACE('',#9769,6.35000000000122);
#8815=CYLINDRICAL_SURFACE('',#9772,6.46290152238551);
#8816=CYLINDRICAL_SURFACE('',#9775,6.4629015223855);
#8817=CYLINDRICAL_SURFACE('',#9778,6.34999999999994);
#8818=CYLINDRICAL_SURFACE('',#9781,6.34999999999994);
#8819=CYLINDRICAL_SURFACE('',#9835,4.);
#8820=CYLINDRICAL_SURFACE('',#9837,4.);
#8821=CYLINDRICAL_SURFACE('',#9838,4.);
#8822=CYLINDRICAL_SURFACE('',#9840,4.);
#8823=CYLINDRICAL_SURFACE('',#9842,4.);
#8824=CYLINDRICAL_SURFACE('',#9846,1.);
#8825=CYLINDRICAL_SURFACE('',#9848,1.);
#8826=CYLINDRICAL_SURFACE('',#9850,1.);
#8827=CYLINDRICAL_SURFACE('',#9851,1.);
#8828=CYLINDRICAL_SURFACE('',#9853,1.);
#8829=CYLINDRICAL_SURFACE('',#9862,4.);
#8830=CYLINDRICAL_SURFACE('',#9863,1.);
#8831=CYLINDRICAL_SURFACE('',#9877,4.);
#8832=CYLINDRICAL_SURFACE('',#9878,1.);
#8833=CYLINDRICAL_SURFACE('',#9887,6.00000000000001);
#8834=CYLINDRICAL_SURFACE('',#9890,6.00000000000001);
#8835=CYLINDRICAL_SURFACE('',#9893,6.00000000000001);
#8836=CYLINDRICAL_SURFACE('',#9896,6.00000000000001);
#8837=CYLINDRICAL_SURFACE('',#9899,6.34999999999994);
#8838=CYLINDRICAL_SURFACE('',#9902,6.34999999999997);
#8839=CYLINDRICAL_SURFACE('',#9905,6.34999999999995);
#8840=CYLINDRICAL_SURFACE('',#9908,6.34999999999997);
#8841=CYLINDRICAL_SURFACE('',#9962,4.);
#8842=CYLINDRICAL_SURFACE('',#9964,4.);
#8843=CYLINDRICAL_SURFACE('',#9966,4.);
#8844=CYLINDRICAL_SURFACE('',#9967,4.);
#8845=CYLINDRICAL_SURFACE('',#9969,4.);
#8846=CYLINDRICAL_SURFACE('',#9973,1.);
#8847=CYLINDRICAL_SURFACE('',#9975,1.);
#8848=CYLINDRICAL_SURFACE('',#9976,1.);
#8849=CYLINDRICAL_SURFACE('',#9978,1.);
#8850=CYLINDRICAL_SURFACE('',#9980,1.);
#8851=CYLINDRICAL_SURFACE('',#9989,4.);
#8852=CYLINDRICAL_SURFACE('',#9990,1.);
#8853=CYLINDRICAL_SURFACE('',#10004,4.);
#8854=CYLINDRICAL_SURFACE('',#10005,1.);
#8855=CYLINDRICAL_SURFACE('',#10014,6.34999999871023);
#8856=CYLINDRICAL_SURFACE('',#10017,6.34999999871025);
#8857=CYLINDRICAL_SURFACE('',#10020,6.34999999999997);
#8858=CYLINDRICAL_SURFACE('',#10023,6.98053323984749);
#8859=CYLINDRICAL_SURFACE('',#10026,6.35);
#8860=CYLINDRICAL_SURFACE('',#10029,6.34999999999999);
#8861=CYLINDRICAL_SURFACE('',#10032,6.35);
#8862=CYLINDRICAL_SURFACE('',#10035,6.35);
#8863=CYLINDRICAL_SURFACE('',#10058,4.);
#8864=CYLINDRICAL_SURFACE('',#10062,4.);
#8865=CYLINDRICAL_SURFACE('',#10064,4.);
#8866=CYLINDRICAL_SURFACE('',#10068,1.);
#8867=CYLINDRICAL_SURFACE('',#10070,1.);
#8868=CYLINDRICAL_SURFACE('',#10072,1.);
#8869=CYLINDRICAL_SURFACE('',#10081,7.11098481470124);
#8870=CYLINDRICAL_SURFACE('',#10084,6.34999999871023);
#8871=CYLINDRICAL_SURFACE('',#10087,6.34999999999997);
#8872=CYLINDRICAL_SURFACE('',#10090,6.98053323984749);
#8873=CYLINDRICAL_SURFACE('',#10093,6.35);
#8874=CYLINDRICAL_SURFACE('',#10096,6.34999999999999);
#8875=CYLINDRICAL_SURFACE('',#10099,6.35);
#8876=CYLINDRICAL_SURFACE('',#10102,6.35);
#8877=CYLINDRICAL_SURFACE('',#10125,4.);
#8878=CYLINDRICAL_SURFACE('',#10129,4.);
#8879=CYLINDRICAL_SURFACE('',#10131,4.);
#8880=CYLINDRICAL_SURFACE('',#10135,1.);
#8881=CYLINDRICAL_SURFACE('',#10137,1.);
#8882=CYLINDRICAL_SURFACE('',#10139,1.);
#8883=CYLINDRICAL_SURFACE('',#10148,6.34999999999999);
#8884=CYLINDRICAL_SURFACE('',#10151,6.34999999999999);
#8885=CYLINDRICAL_SURFACE('',#10154,6.35);
#8886=CYLINDRICAL_SURFACE('',#10185,1.);
#8887=CYLINDRICAL_SURFACE('',#10189,5.7625);
#8888=CYLINDRICAL_SURFACE('',#10191,5.7625);
#8889=CYLINDRICAL_SURFACE('',#10193,1.);
#8890=CYLINDRICAL_SURFACE('',#10197,5.7625);
#8891=CYLINDRICAL_SURFACE('',#10199,1.);
#8892=CYLINDRICAL_SURFACE('',#10201,1.);
#8893=CYLINDRICAL_SURFACE('',#10203,5.7625);
#8894=CYLINDRICAL_SURFACE('',#10231,4.);
#8895=CYLINDRICAL_SURFACE('',#10233,4.);
#8896=CYLINDRICAL_SURFACE('',#10237,1.);
#8897=CYLINDRICAL_SURFACE('',#10239,1.);
#8898=CYLINDRICAL_SURFACE('',#10248,26.924);
#8899=CYLINDRICAL_SURFACE('',#10300,0.360879621470698);
#8900=CYLINDRICAL_SURFACE('',#10301,0.166559825294127);
#8901=CYLINDRICAL_SURFACE('',#10302,0.360879621470687);
#8902=CYLINDRICAL_SURFACE('',#10303,0.166559825294309);
#8903=CYLINDRICAL_SURFACE('',#10304,0.166559825294299);
#8904=CYLINDRICAL_SURFACE('',#10305,0.360879621470696);
#8905=CYLINDRICAL_SURFACE('',#10306,0.360879621470822);
#8906=CYLINDRICAL_SURFACE('',#10307,0.166559825294181);
#8907=CYLINDRICAL_SURFACE('',#10308,0.360879621470762);
#8908=CYLINDRICAL_SURFACE('',#10309,0.166559825294205);
#8909=CYLINDRICAL_SURFACE('',#10310,10.922);
#8910=CYLINDRICAL_SURFACE('',#10316,24.384);
#8911=CYLINDRICAL_SURFACE('',#10318,3.24485);
#8912=CYLINDRICAL_SURFACE('',#10321,4.03225);
#8913=CYLINDRICAL_SURFACE('',#10330,11.1252);
#8914=CYLINDRICAL_SURFACE('',#10333,11.1252);
#8915=CYLINDRICAL_SURFACE('',#10337,3.175);
#8916=CYLINDRICAL_SURFACE('',#10338,3.175);
#8917=CYLINDRICAL_SURFACE('',#10339,3.175);
#8918=CYLINDRICAL_SURFACE('',#10340,3.175);
#8919=CYLINDRICAL_SURFACE('',#10344,0.166559825294142);
#8920=CYLINDRICAL_SURFACE('',#10347,0.16655982529419);
#8921=CYLINDRICAL_SURFACE('',#10350,0.360879621470784);
#8922=CYLINDRICAL_SURFACE('',#10351,0.360879621470672);
#8923=CYLINDRICAL_SURFACE('',#10352,0.166559825294127);
#8924=CYLINDRICAL_SURFACE('',#10359,0.166559825294242);
#8925=CYLINDRICAL_SURFACE('',#10364,0.36087962147082);
#8926=CYLINDRICAL_SURFACE('',#10365,0.360879621470515);
#8927=CYLINDRICAL_SURFACE('',#10384,26.0773333333334);
#8928=CYLINDRICAL_SURFACE('',#10385,0.360879621470804);
#8929=CYLINDRICAL_SURFACE('',#10386,0.360879621470817);
#8930=CYLINDRICAL_SURFACE('',#10387,0.360879621470515);
#8931=CYLINDRICAL_SURFACE('',#10396,26.0773333333334);
#8932=CYLINDRICAL_SURFACE('',#10405,0.166559825294052);
#8933=CYLINDRICAL_SURFACE('',#10408,0.1665598252943);
#8934=CYLINDRICAL_SURFACE('',#10411,0.166559825294036);
#8935=CYLINDRICAL_SURFACE('',#10412,26.924);
#8936=CYLINDRICAL_SURFACE('',#10413,0.360879621470804);
#8937=CYLINDRICAL_SURFACE('',#10414,0.360879621470665);
#8938=CYLINDRICAL_SURFACE('',#10415,0.166559825294133);
#8939=CYLINDRICAL_SURFACE('',#10422,0.166559825294394);
#8940=CYLINDRICAL_SURFACE('',#10427,0.166559825293995);
#8941=CYLINDRICAL_SURFACE('',#10430,0.36087962147052);
#8942=CYLINDRICAL_SURFACE('',#10443,26.0773333333334);
#8943=CYLINDRICAL_SURFACE('',#10444,0.360879621470749);
#8944=CYLINDRICAL_SURFACE('',#10445,0.360879621470817);
#8945=CYLINDRICAL_SURFACE('',#10446,0.166559825294108);
#8946=CYLINDRICAL_SURFACE('',#10453,0.166559825294446);
#8947=CYLINDRICAL_SURFACE('',#10468,26.0773333333334);
#8948=CYLINDRICAL_SURFACE('',#10477,26.0773333333334);
#8949=CYLINDRICAL_SURFACE('',#10481,0.166559825294076);
#8950=CYLINDRICAL_SURFACE('',#10485,0.166559825294277);
#8951=CYLINDRICAL_SURFACE('',#10489,0.166559825294382);
#8952=CYLINDRICAL_SURFACE('',#10493,26.924);
#8953=CYLINDRICAL_SURFACE('',#10494,26.0773333333334);
#8954=CYLINDRICAL_SURFACE('',#10503,0.360879621470515);
#8955=CYLINDRICAL_SURFACE('',#10504,0.360879621470817);
#8956=CYLINDRICAL_SURFACE('',#10505,0.360879621470782);
#8957=CYLINDRICAL_SURFACE('',#10513,3.9243);
#8958=CYLINDRICAL_SURFACE('',#10518,3.175);
#8959=CYLINDRICAL_SURFACE('',#10547,5.6515);
#8960=CYLINDRICAL_SURFACE('',#10564,19.05);
#8961=CYLINDRICAL_SURFACE('',#10593,5.4991);
#8962=CYLINDRICAL_SURFACE('',#10605,2.48793);
#8963=CYLINDRICAL_SURFACE('',#10648,5.55625);
#8964=CYLINDRICAL_SURFACE('',#10654,3.5687);
#8965=CYLINDRICAL_SURFACE('',#10656,5.55625);
#8966=CYLINDRICAL_SURFACE('',#10661,9.525);
#8967=CYLINDRICAL_SURFACE('',#10671,5.4991);
#8968=CYLINDRICAL_SURFACE('',#10692,5.6388);
#8969=CYLINDRICAL_SURFACE('',#10740,39.751);
#8970=CYLINDRICAL_SURFACE('',#10747,45.30725);
#8971=CYLINDRICAL_SURFACE('',#10752,39.751);
#8972=CYLINDRICAL_SURFACE('',#10761,7.7216);
#8973=CYLINDRICAL_SURFACE('',#10773,39.751);
#8974=CYLINDRICAL_SURFACE('',#10780,45.30725);
#8975=CYLINDRICAL_SURFACE('',#10785,39.751);
#8976=CYLINDRICAL_SURFACE('',#10818,4.0386);
#8977=CYLINDRICAL_SURFACE('',#10821,5.55625);
#8978=CYLINDRICAL_SURFACE('',#10831,5.6515);
#8979=CYLINDRICAL_SURFACE('',#10835,7.6835);
#8980=ADVANCED_FACE('',(#841),#8808,.F.);
#8981=ADVANCED_FACE('',(#842),#8809,.F.);
#8982=ADVANCED_FACE('',(#843),#8810,.F.);
#8983=ADVANCED_FACE('',(#844),#8811,.F.);
#8984=ADVANCED_FACE('',(#845),#8812,.F.);
#8985=ADVANCED_FACE('',(#846),#8813,.F.);
#8986=ADVANCED_FACE('',(#847),#8814,.F.);
#8987=ADVANCED_FACE('',(#848),#8815,.F.);
#8988=ADVANCED_FACE('',(#849),#8816,.F.);
#8989=ADVANCED_FACE('',(#850),#8817,.F.);
#8990=ADVANCED_FACE('',(#851),#8818,.F.);
#8991=ADVANCED_FACE('',(#852),#502,.T.);
#8992=ADVANCED_FACE('',(#853),#503,.T.);
#8993=ADVANCED_FACE('',(#854),#504,.T.);
#8994=ADVANCED_FACE('',(#855),#505,.F.);
#8995=ADVANCED_FACE('',(#856),#506,.T.);
#8996=ADVANCED_FACE('',(#857),#507,.T.);
#8997=ADVANCED_FACE('',(#858),#508,.T.);
#8998=ADVANCED_FACE('',(#859),#509,.T.);
#8999=ADVANCED_FACE('',(#860),#510,.T.);
#9000=ADVANCED_FACE('',(#861),#511,.T.);
#9001=ADVANCED_FACE('',(#862),#512,.T.);
#9002=ADVANCED_FACE('',(#863),#513,.T.);
#9003=ADVANCED_FACE('',(#864),#514,.T.);
#9004=ADVANCED_FACE('',(#865),#515,.T.);
#9005=ADVANCED_FACE('',(#866),#516,.T.);
#9006=ADVANCED_FACE('',(#867),#517,.T.);
#9007=ADVANCED_FACE('',(#868),#518,.T.);
#9008=ADVANCED_FACE('',(#869),#519,.T.);
#9009=ADVANCED_FACE('',(#870),#520,.T.);
#9010=ADVANCED_FACE('',(#871),#521,.T.);
#9011=ADVANCED_FACE('',(#872),#522,.T.);
#9012=ADVANCED_FACE('',(#873),#523,.T.);
#9013=ADVANCED_FACE('',(#874),#524,.T.);
#9014=ADVANCED_FACE('',(#875),#525,.T.);
#9015=ADVANCED_FACE('',(#876,#379,#380,#381,#382),#526,.F.);
#9016=ADVANCED_FACE('',(#877),#527,.T.);
#9017=ADVANCED_FACE('',(#878,#383,#384,#385,#386),#528,.T.);
#9018=ADVANCED_FACE('',(#879),#8819,.T.);
#9019=ADVANCED_FACE('',(#880),#529,.T.);
#9020=ADVANCED_FACE('',(#881),#8820,.T.);
#9021=ADVANCED_FACE('',(#882),#8821,.T.);
#9022=ADVANCED_FACE('',(#883),#530,.T.);
#9023=ADVANCED_FACE('',(#884),#8822,.T.);
#9024=ADVANCED_FACE('',(#885),#531,.T.);
#9025=ADVANCED_FACE('',(#886),#8823,.T.);
#9026=ADVANCED_FACE('',(#887,#387,#388,#389),#532,.T.);
#9027=ADVANCED_FACE('',(#888),#533,.T.);
#9028=ADVANCED_FACE('',(#889,#390,#391,#392),#534,.F.);
#9029=ADVANCED_FACE('',(#890),#8824,.F.);
#9030=ADVANCED_FACE('',(#891),#535,.F.);
#9031=ADVANCED_FACE('',(#892),#8825,.F.);
#9032=ADVANCED_FACE('',(#893),#536,.F.);
#9033=ADVANCED_FACE('',(#894),#8826,.F.);
#9034=ADVANCED_FACE('',(#895),#8827,.F.);
#9035=ADVANCED_FACE('',(#896),#537,.F.);
#9036=ADVANCED_FACE('',(#897),#8828,.F.);
#9037=ADVANCED_FACE('',(#898),#538,.T.);
#9038=ADVANCED_FACE('',(#899),#539,.F.);
#9039=ADVANCED_FACE('',(#900),#540,.T.);
#9040=ADVANCED_FACE('',(#901),#541,.F.);
#9041=ADVANCED_FACE('',(#902),#8829,.T.);
#9042=ADVANCED_FACE('',(#903),#8830,.F.);
#9043=ADVANCED_FACE('',(#904),#542,.F.);
#9044=ADVANCED_FACE('',(#905),#543,.F.);
#9045=ADVANCED_FACE('',(#906,#393,#394),#544,.F.);
#9046=ADVANCED_FACE('',(#907,#395,#396),#545,.T.);
#9047=ADVANCED_FACE('',(#908),#546,.F.);
#9048=ADVANCED_FACE('',(#909),#547,.T.);
#9049=ADVANCED_FACE('',(#910),#548,.T.);
#9050=ADVANCED_FACE('',(#911),#549,.T.);
#9051=ADVANCED_FACE('',(#912),#550,.F.);
#9052=ADVANCED_FACE('',(#913),#8831,.T.);
#9053=ADVANCED_FACE('',(#914),#8832,.F.);
#9054=ADVANCED_FACE('',(#915),#551,.F.);
#9055=ADVANCED_FACE('',(#916),#552,.F.);
#9056=ADVANCED_FACE('',(#917,#397,#398),#553,.F.);
#9057=ADVANCED_FACE('',(#918,#399,#400),#554,.T.);
#9058=ADVANCED_FACE('',(#919),#555,.F.);
#9059=ADVANCED_FACE('',(#920),#556,.T.);
#9060=ADVANCED_FACE('',(#921),#557,.T.);
#9061=ADVANCED_FACE('',(#922),#8833,.F.);
#9062=ADVANCED_FACE('',(#923),#8834,.F.);
#9063=ADVANCED_FACE('',(#924),#8835,.F.);
#9064=ADVANCED_FACE('',(#925),#8836,.F.);
#9065=ADVANCED_FACE('',(#926),#8837,.F.);
#9066=ADVANCED_FACE('',(#927),#8838,.F.);
#9067=ADVANCED_FACE('',(#928),#8839,.F.);
#9068=ADVANCED_FACE('',(#929),#8840,.F.);
#9069=ADVANCED_FACE('',(#930),#558,.T.);
#9070=ADVANCED_FACE('',(#931),#559,.T.);
#9071=ADVANCED_FACE('',(#932),#560,.T.);
#9072=ADVANCED_FACE('',(#933),#561,.F.);
#9073=ADVANCED_FACE('',(#934),#562,.T.);
#9074=ADVANCED_FACE('',(#935),#563,.T.);
#9075=ADVANCED_FACE('',(#936),#564,.T.);
#9076=ADVANCED_FACE('',(#937),#565,.T.);
#9077=ADVANCED_FACE('',(#938),#566,.T.);
#9078=ADVANCED_FACE('',(#939),#567,.T.);
#9079=ADVANCED_FACE('',(#940),#568,.T.);
#9080=ADVANCED_FACE('',(#941),#569,.T.);
#9081=ADVANCED_FACE('',(#942),#570,.T.);
#9082=ADVANCED_FACE('',(#943),#571,.T.);
#9083=ADVANCED_FACE('',(#944),#572,.T.);
#9084=ADVANCED_FACE('',(#945),#573,.T.);
#9085=ADVANCED_FACE('',(#946),#574,.T.);
#9086=ADVANCED_FACE('',(#947),#575,.T.);
#9087=ADVANCED_FACE('',(#948),#576,.T.);
#9088=ADVANCED_FACE('',(#949),#577,.T.);
#9089=ADVANCED_FACE('',(#950),#578,.T.);
#9090=ADVANCED_FACE('',(#951),#579,.T.);
#9091=ADVANCED_FACE('',(#952),#580,.T.);
#9092=ADVANCED_FACE('',(#953),#581,.T.);
#9093=ADVANCED_FACE('',(#954,#401,#402),#582,.F.);
#9094=ADVANCED_FACE('',(#955),#583,.T.);
#9095=ADVANCED_FACE('',(#956,#403,#404),#584,.T.);
#9096=ADVANCED_FACE('',(#957),#8841,.T.);
#9097=ADVANCED_FACE('',(#958),#585,.T.);
#9098=ADVANCED_FACE('',(#959),#8842,.T.);
#9099=ADVANCED_FACE('',(#960),#586,.T.);
#9100=ADVANCED_FACE('',(#961),#8843,.T.);
#9101=ADVANCED_FACE('',(#962),#8844,.T.);
#9102=ADVANCED_FACE('',(#963),#587,.T.);
#9103=ADVANCED_FACE('',(#964),#8845,.T.);
#9104=ADVANCED_FACE('',(#965,#405,#406),#588,.T.);
#9105=ADVANCED_FACE('',(#966),#589,.T.);
#9106=ADVANCED_FACE('',(#967,#407,#408),#590,.F.);
#9107=ADVANCED_FACE('',(#968),#8846,.F.);
#9108=ADVANCED_FACE('',(#969),#591,.F.);
#9109=ADVANCED_FACE('',(#970),#8847,.F.);
#9110=ADVANCED_FACE('',(#971),#8848,.F.);
#9111=ADVANCED_FACE('',(#972),#592,.F.);
#9112=ADVANCED_FACE('',(#973),#8849,.F.);
#9113=ADVANCED_FACE('',(#974),#593,.F.);
#9114=ADVANCED_FACE('',(#975),#8850,.F.);
#9115=ADVANCED_FACE('',(#976),#594,.T.);
#9116=ADVANCED_FACE('',(#977),#595,.F.);
#9117=ADVANCED_FACE('',(#978),#596,.T.);
#9118=ADVANCED_FACE('',(#979),#597,.F.);
#9119=ADVANCED_FACE('',(#980),#8851,.T.);
#9120=ADVANCED_FACE('',(#981),#8852,.F.);
#9121=ADVANCED_FACE('',(#982),#598,.F.);
#9122=ADVANCED_FACE('',(#983),#599,.F.);
#9123=ADVANCED_FACE('',(#984,#409,#410),#600,.F.);
#9124=ADVANCED_FACE('',(#985,#411,#412),#601,.T.);
#9125=ADVANCED_FACE('',(#986),#602,.F.);
#9126=ADVANCED_FACE('',(#987),#603,.T.);
#9127=ADVANCED_FACE('',(#988),#604,.T.);
#9128=ADVANCED_FACE('',(#989),#605,.T.);
#9129=ADVANCED_FACE('',(#990),#606,.F.);
#9130=ADVANCED_FACE('',(#991),#8853,.T.);
#9131=ADVANCED_FACE('',(#992),#8854,.F.);
#9132=ADVANCED_FACE('',(#993),#607,.F.);
#9133=ADVANCED_FACE('',(#994),#608,.F.);
#9134=ADVANCED_FACE('',(#995,#413,#414),#609,.F.);
#9135=ADVANCED_FACE('',(#996,#415,#416),#610,.T.);
#9136=ADVANCED_FACE('',(#997),#611,.F.);
#9137=ADVANCED_FACE('',(#998),#612,.T.);
#9138=ADVANCED_FACE('',(#999),#613,.T.);
#9139=ADVANCED_FACE('',(#1000),#8855,.F.);
#9140=ADVANCED_FACE('',(#1001),#8856,.F.);
#9141=ADVANCED_FACE('',(#1002),#8857,.F.);
#9142=ADVANCED_FACE('',(#1003),#8858,.F.);
#9143=ADVANCED_FACE('',(#1004),#8859,.F.);
#9144=ADVANCED_FACE('',(#1005),#8860,.F.);
#9145=ADVANCED_FACE('',(#1006),#8861,.F.);
#9146=ADVANCED_FACE('',(#1007),#8862,.F.);
#9147=ADVANCED_FACE('',(#1008),#614,.T.);
#9148=ADVANCED_FACE('',(#1009),#615,.T.);
#9149=ADVANCED_FACE('',(#1010),#616,.T.);
#9150=ADVANCED_FACE('',(#1011),#617,.T.);
#9151=ADVANCED_FACE('',(#1012),#618,.T.);
#9152=ADVANCED_FACE('',(#1013),#619,.T.);
#9153=ADVANCED_FACE('',(#1014),#620,.T.);
#9154=ADVANCED_FACE('',(#1015),#621,.T.);
#9155=ADVANCED_FACE('',(#1016),#622,.T.);
#9156=ADVANCED_FACE('',(#1017),#623,.F.);
#9157=ADVANCED_FACE('',(#1018),#624,.T.);
#9158=ADVANCED_FACE('',(#1019),#625,.T.);
#9159=ADVANCED_FACE('',(#1020),#8863,.T.);
#9160=ADVANCED_FACE('',(#1021),#626,.T.);
#9161=ADVANCED_FACE('',(#1022),#8864,.T.);
#9162=ADVANCED_FACE('',(#1023,#417,#418,#419,#420),#627,.T.);
#9163=ADVANCED_FACE('',(#1024),#8865,.T.);
#9164=ADVANCED_FACE('',(#1025,#421,#422,#423,#424),#628,.T.);
#9165=ADVANCED_FACE('',(#1026),#629,.T.);
#9166=ADVANCED_FACE('',(#1027,#425,#426,#427,#428),#630,.F.);
#9167=ADVANCED_FACE('',(#1028),#8866,.F.);
#9168=ADVANCED_FACE('',(#1029,#429,#430,#431,#432),#631,.F.);
#9169=ADVANCED_FACE('',(#1030),#8867,.F.);
#9170=ADVANCED_FACE('',(#1031),#632,.F.);
#9171=ADVANCED_FACE('',(#1032),#8868,.F.);
#9172=ADVANCED_FACE('',(#1033),#633,.F.);
#9173=ADVANCED_FACE('',(#1034),#634,.F.);
#9174=ADVANCED_FACE('',(#1035),#635,.F.);
#9175=ADVANCED_FACE('',(#1036),#636,.F.);
#9176=ADVANCED_FACE('',(#1037),#637,.T.);
#9177=ADVANCED_FACE('',(#1038),#8869,.F.);
#9178=ADVANCED_FACE('',(#1039),#8870,.F.);
#9179=ADVANCED_FACE('',(#1040),#8871,.F.);
#9180=ADVANCED_FACE('',(#1041),#8872,.F.);
#9181=ADVANCED_FACE('',(#1042),#8873,.F.);
#9182=ADVANCED_FACE('',(#1043),#8874,.F.);
#9183=ADVANCED_FACE('',(#1044),#8875,.F.);
#9184=ADVANCED_FACE('',(#1045),#8876,.F.);
#9185=ADVANCED_FACE('',(#1046),#638,.T.);
#9186=ADVANCED_FACE('',(#1047),#639,.T.);
#9187=ADVANCED_FACE('',(#1048),#640,.T.);
#9188=ADVANCED_FACE('',(#1049),#641,.T.);
#9189=ADVANCED_FACE('',(#1050),#642,.T.);
#9190=ADVANCED_FACE('',(#1051),#643,.T.);
#9191=ADVANCED_FACE('',(#1052),#644,.T.);
#9192=ADVANCED_FACE('',(#1053),#645,.T.);
#9193=ADVANCED_FACE('',(#1054),#646,.T.);
#9194=ADVANCED_FACE('',(#1055),#647,.F.);
#9195=ADVANCED_FACE('',(#1056),#648,.T.);
#9196=ADVANCED_FACE('',(#1057),#649,.T.);
#9197=ADVANCED_FACE('',(#1058),#8877,.T.);
#9198=ADVANCED_FACE('',(#1059),#650,.T.);
#9199=ADVANCED_FACE('',(#1060),#8878,.T.);
#9200=ADVANCED_FACE('',(#1061,#433,#434,#435,#436),#651,.T.);
#9201=ADVANCED_FACE('',(#1062),#8879,.T.);
#9202=ADVANCED_FACE('',(#1063,#437,#438,#439,#440),#652,.T.);
#9203=ADVANCED_FACE('',(#1064),#653,.T.);
#9204=ADVANCED_FACE('',(#1065,#441,#442,#443,#444),#654,.F.);
#9205=ADVANCED_FACE('',(#1066),#8880,.F.);
#9206=ADVANCED_FACE('',(#1067,#445,#446,#447,#448),#655,.F.);
#9207=ADVANCED_FACE('',(#1068),#8881,.F.);
#9208=ADVANCED_FACE('',(#1069),#656,.F.);
#9209=ADVANCED_FACE('',(#1070),#8882,.F.);
#9210=ADVANCED_FACE('',(#1071),#657,.F.);
#9211=ADVANCED_FACE('',(#1072),#658,.F.);
#9212=ADVANCED_FACE('',(#1073),#659,.F.);
#9213=ADVANCED_FACE('',(#1074),#660,.F.);
#9214=ADVANCED_FACE('',(#1075),#661,.T.);
#9215=ADVANCED_FACE('',(#1076),#8883,.F.);
#9216=ADVANCED_FACE('',(#1077),#8884,.F.);
#9217=ADVANCED_FACE('',(#1078),#8885,.F.);
#9218=ADVANCED_FACE('',(#1079),#662,.T.);
#9219=ADVANCED_FACE('',(#1080),#663,.T.);
#9220=ADVANCED_FACE('',(#1081),#664,.T.);
#9221=ADVANCED_FACE('',(#1082),#665,.T.);
#9222=ADVANCED_FACE('',(#1083),#666,.T.);
#9223=ADVANCED_FACE('',(#1084),#667,.T.);
#9224=ADVANCED_FACE('',(#1085),#668,.T.);
#9225=ADVANCED_FACE('',(#1086),#669,.T.);
#9226=ADVANCED_FACE('',(#1087),#670,.T.);
#9227=ADVANCED_FACE('',(#1088),#671,.T.);
#9228=ADVANCED_FACE('',(#1089),#672,.T.);
#9229=ADVANCED_FACE('',(#1090),#673,.T.);
#9230=ADVANCED_FACE('',(#1091),#674,.T.);
#9231=ADVANCED_FACE('',(#1092),#675,.F.);
#9232=ADVANCED_FACE('',(#1093),#676,.T.);
#9233=ADVANCED_FACE('',(#1094),#677,.T.);
#9234=ADVANCED_FACE('',(#1095),#8886,.F.);
#9235=ADVANCED_FACE('',(#1096),#678,.T.);
#9236=ADVANCED_FACE('',(#1097),#8887,.T.);
#9237=ADVANCED_FACE('',(#1098),#679,.T.);
#9238=ADVANCED_FACE('',(#1099),#8888,.T.);
#9239=ADVANCED_FACE('',(#1100),#680,.T.);
#9240=ADVANCED_FACE('',(#1101),#8889,.F.);
#9241=ADVANCED_FACE('',(#1102,#449,#450,#451),#681,.T.);
#9242=ADVANCED_FACE('',(#1103),#682,.T.);
#9243=ADVANCED_FACE('',(#1104,#452,#453,#454),#683,.F.);
#9244=ADVANCED_FACE('',(#1105),#8890,.T.);
#9245=ADVANCED_FACE('',(#1106),#684,.F.);
#9246=ADVANCED_FACE('',(#1107),#8891,.F.);
#9247=ADVANCED_FACE('',(#1108),#685,.F.);
#9248=ADVANCED_FACE('',(#1109),#8892,.F.);
#9249=ADVANCED_FACE('',(#1110),#686,.F.);
#9250=ADVANCED_FACE('',(#1111),#8893,.T.);
#9251=ADVANCED_FACE('',(#1112),#687,.F.);
#9252=ADVANCED_FACE('',(#1113),#688,.F.);
#9253=ADVANCED_FACE('',(#1114),#689,.F.);
#9254=ADVANCED_FACE('',(#1115),#690,.F.);
#9255=ADVANCED_FACE('',(#1116),#691,.F.);
#9256=ADVANCED_FACE('',(#1117),#692,.T.);
#9257=ADVANCED_FACE('',(#1118),#693,.T.);
#9258=ADVANCED_FACE('',(#1119),#694,.T.);
#9259=ADVANCED_FACE('',(#1120),#695,.T.);
#9260=ADVANCED_FACE('',(#1121),#696,.T.);
#9261=ADVANCED_FACE('',(#1122),#697,.T.);
#9262=ADVANCED_FACE('',(#1123),#698,.T.);
#9263=ADVANCED_FACE('',(#1124),#699,.T.);
#9264=ADVANCED_FACE('',(#1125),#700,.F.);
#9265=ADVANCED_FACE('',(#1126),#701,.T.);
#9266=ADVANCED_FACE('',(#1127),#702,.T.);
#9267=ADVANCED_FACE('',(#1128),#8894,.T.);
#9268=ADVANCED_FACE('',(#1129),#703,.T.);
#9269=ADVANCED_FACE('',(#1130),#8895,.T.);
#9270=ADVANCED_FACE('',(#1131),#704,.T.);
#9271=ADVANCED_FACE('',(#1132),#705,.T.);
#9272=ADVANCED_FACE('',(#1133),#706,.F.);
#9273=ADVANCED_FACE('',(#1134),#8896,.F.);
#9274=ADVANCED_FACE('',(#1135),#707,.F.);
#9275=ADVANCED_FACE('',(#1136),#8897,.F.);
#9276=ADVANCED_FACE('',(#1137),#708,.T.);
#9277=ADVANCED_FACE('',(#1138),#709,.F.);
#9278=ADVANCED_FACE('',(#1139),#237,.T.);
#9279=ADVANCED_FACE('',(#1140,#455,#456,#457,#458,#459,#460),#8898,.T.);
#9280=ADVANCED_FACE('',(#1141),#8899,.F.);
#9281=ADVANCED_FACE('',(#1142),#8900,.T.);
#9282=ADVANCED_FACE('',(#1143),#8901,.F.);
#9283=ADVANCED_FACE('',(#1144),#8902,.T.);
#9284=ADVANCED_FACE('',(#1145),#8903,.T.);
#9285=ADVANCED_FACE('',(#1146),#8904,.F.);
#9286=ADVANCED_FACE('',(#1147),#8905,.F.);
#9287=ADVANCED_FACE('',(#1148),#8906,.T.);
#9288=ADVANCED_FACE('',(#1149),#8907,.F.);
#9289=ADVANCED_FACE('',(#1150),#8908,.T.);
#9290=ADVANCED_FACE('',(#1151),#8909,.F.);
#9291=ADVANCED_FACE('',(#1152),#238,.F.);
#9292=ADVANCED_FACE('',(#1153),#8910,.F.);
#9293=ADVANCED_FACE('',(#1154),#8911,.F.);
#9294=ADVANCED_FACE('',(#1155),#8912,.F.);
#9295=ADVANCED_FACE('',(#1156),#710,.F.);
#9296=ADVANCED_FACE('',(#1157),#711,.F.);
#9297=ADVANCED_FACE('',(#1158),#8913,.T.);
#9298=ADVANCED_FACE('',(#1159),#8914,.T.);
#9299=ADVANCED_FACE('',(#1160,#461),#712,.T.);
#9300=ADVANCED_FACE('',(#1161),#8915,.F.);
#9301=ADVANCED_FACE('',(#1162),#8916,.F.);
#9302=ADVANCED_FACE('',(#1163),#8917,.T.);
#9303=ADVANCED_FACE('',(#1164),#8918,.T.);
#9304=ADVANCED_FACE('',(#1165,#462),#713,.F.);
#9305=ADVANCED_FACE('',(#1166,#463),#714,.F.);
#9306=ADVANCED_FACE('',(#1167,#464),#715,.F.);
#9307=ADVANCED_FACE('',(#1168),#8919,.T.);
#9308=ADVANCED_FACE('',(#1169),#716,.T.);
#9309=ADVANCED_FACE('',(#1170),#8920,.T.);
#9310=ADVANCED_FACE('',(#1171),#717,.T.);
#9311=ADVANCED_FACE('',(#1172),#8921,.F.);
#9312=ADVANCED_FACE('',(#1173),#8922,.F.);
#9313=ADVANCED_FACE('',(#1174),#8923,.T.);
#9314=ADVANCED_FACE('',(#1175),#718,.T.);
#9315=ADVANCED_FACE('',(#1176),#719,.T.);
#9316=ADVANCED_FACE('',(#1177),#720,.T.);
#9317=ADVANCED_FACE('',(#1178),#8924,.T.);
#9318=ADVANCED_FACE('',(#1179),#721,.T.);
#9319=ADVANCED_FACE('',(#1180),#722,.T.);
#9320=ADVANCED_FACE('',(#1181),#8925,.F.);
#9321=ADVANCED_FACE('',(#1182),#8926,.F.);
#9322=ADVANCED_FACE('',(#1183),#723,.T.);
#9323=ADVANCED_FACE('',(#1184),#724,.T.);
#9324=ADVANCED_FACE('',(#1185),#725,.T.);
#9325=ADVANCED_FACE('',(#1186),#726,.T.);
#9326=ADVANCED_FACE('',(#1187),#727,.T.);
#9327=ADVANCED_FACE('',(#1188),#728,.T.);
#9328=ADVANCED_FACE('',(#1189),#729,.T.);
#9329=ADVANCED_FACE('',(#1190),#730,.T.);
#9330=ADVANCED_FACE('',(#1191),#731,.T.);
#9331=ADVANCED_FACE('',(#1192),#8927,.T.);
#9332=ADVANCED_FACE('',(#1193),#8928,.F.);
#9333=ADVANCED_FACE('',(#1194),#8929,.F.);
#9334=ADVANCED_FACE('',(#1195),#8930,.F.);
#9335=ADVANCED_FACE('',(#1196),#732,.T.);
#9336=ADVANCED_FACE('',(#1197),#733,.T.);
#9337=ADVANCED_FACE('',(#1198),#734,.T.);
#9338=ADVANCED_FACE('',(#1199),#735,.T.);
#9339=ADVANCED_FACE('',(#1200,#465),#8931,.T.);
#9340=ADVANCED_FACE('',(#1201),#736,.F.);
#9341=ADVANCED_FACE('',(#1202),#737,.F.);
#9342=ADVANCED_FACE('',(#1203),#8932,.T.);
#9343=ADVANCED_FACE('',(#1204),#738,.F.);
#9344=ADVANCED_FACE('',(#1205),#8933,.T.);
#9345=ADVANCED_FACE('',(#1206),#739,.F.);
#9346=ADVANCED_FACE('',(#1207),#8934,.T.);
#9347=ADVANCED_FACE('',(#1208),#8935,.T.);
#9348=ADVANCED_FACE('',(#1209),#8936,.F.);
#9349=ADVANCED_FACE('',(#1210),#8937,.F.);
#9350=ADVANCED_FACE('',(#1211),#8938,.T.);
#9351=ADVANCED_FACE('',(#1212),#740,.T.);
#9352=ADVANCED_FACE('',(#1213),#741,.T.);
#9353=ADVANCED_FACE('',(#1214),#742,.T.);
#9354=ADVANCED_FACE('',(#1215),#8939,.T.);
#9355=ADVANCED_FACE('',(#1216),#743,.T.);
#9356=ADVANCED_FACE('',(#1217),#744,.T.);
#9357=ADVANCED_FACE('',(#1218),#8940,.T.);
#9358=ADVANCED_FACE('',(#1219),#745,.T.);
#9359=ADVANCED_FACE('',(#1220),#8941,.F.);
#9360=ADVANCED_FACE('',(#1221),#746,.T.);
#9361=ADVANCED_FACE('',(#1222),#747,.T.);
#9362=ADVANCED_FACE('',(#1223),#748,.T.);
#9363=ADVANCED_FACE('',(#1224),#749,.T.);
#9364=ADVANCED_FACE('',(#1225),#750,.T.);
#9365=ADVANCED_FACE('',(#1226),#751,.T.);
#9366=ADVANCED_FACE('',(#1227),#8942,.T.);
#9367=ADVANCED_FACE('',(#1228),#8943,.F.);
#9368=ADVANCED_FACE('',(#1229),#8944,.F.);
#9369=ADVANCED_FACE('',(#1230),#8945,.T.);
#9370=ADVANCED_FACE('',(#1231),#752,.T.);
#9371=ADVANCED_FACE('',(#1232),#753,.T.);
#9372=ADVANCED_FACE('',(#1233),#754,.T.);
#9373=ADVANCED_FACE('',(#1234),#8946,.T.);
#9374=ADVANCED_FACE('',(#1235),#755,.T.);
#9375=ADVANCED_FACE('',(#1236),#756,.T.);
#9376=ADVANCED_FACE('',(#1237),#757,.T.);
#9377=ADVANCED_FACE('',(#1238),#758,.T.);
#9378=ADVANCED_FACE('',(#1239),#759,.T.);
#9379=ADVANCED_FACE('',(#1240),#760,.T.);
#9380=ADVANCED_FACE('',(#1241),#761,.T.);
#9381=ADVANCED_FACE('',(#1242),#8947,.T.);
#9382=ADVANCED_FACE('',(#1243),#762,.T.);
#9383=ADVANCED_FACE('',(#1244),#763,.T.);
#9384=ADVANCED_FACE('',(#1245),#764,.T.);
#9385=ADVANCED_FACE('',(#1246),#765,.T.);
#9386=ADVANCED_FACE('',(#1247),#8948,.T.);
#9387=ADVANCED_FACE('',(#1248),#766,.F.);
#9388=ADVANCED_FACE('',(#1249),#8949,.T.);
#9389=ADVANCED_FACE('',(#1250),#767,.F.);
#9390=ADVANCED_FACE('',(#1251),#8950,.T.);
#9391=ADVANCED_FACE('',(#1252),#768,.F.);
#9392=ADVANCED_FACE('',(#1253),#8951,.T.);
#9393=ADVANCED_FACE('',(#1254),#769,.F.);
#9394=ADVANCED_FACE('',(#1255),#8952,.T.);
#9395=ADVANCED_FACE('',(#1256,#466),#8953,.T.);
#9396=ADVANCED_FACE('',(#1257),#770,.T.);
#9397=ADVANCED_FACE('',(#1258),#771,.T.);
#9398=ADVANCED_FACE('',(#1259),#772,.T.);
#9399=ADVANCED_FACE('',(#1260),#773,.T.);
#9400=ADVANCED_FACE('',(#1261),#8954,.F.);
#9401=ADVANCED_FACE('',(#1262),#8955,.F.);
#9402=ADVANCED_FACE('',(#1263),#8956,.F.);
#9403=ADVANCED_FACE('',(#1264,#467),#774,.T.);
#9404=ADVANCED_FACE('',(#1265,#468),#775,.T.);
#9405=ADVANCED_FACE('',(#1266),#239,.F.);
#9406=ADVANCED_FACE('',(#1267),#8957,.T.);
#9407=ADVANCED_FACE('',(#1268),#240,.T.);
#9408=ADVANCED_FACE('',(#1269),#8958,.T.);
#9409=ADVANCED_FACE('',(#1270),#119,.T.);
#9410=ADVANCED_FACE('',(#1271),#120,.T.);
#9411=ADVANCED_FACE('',(#1272),#776,.F.);
#9412=ADVANCED_FACE('',(#1273),#121,.T.);
#9413=ADVANCED_FACE('',(#1274),#122,.T.);
#9414=ADVANCED_FACE('',(#1275),#123,.T.);
#9415=ADVANCED_FACE('',(#1276),#124,.T.);
#9416=ADVANCED_FACE('',(#1277),#125,.T.);
#9417=ADVANCED_FACE('',(#1278),#777,.F.);
#9418=ADVANCED_FACE('',(#1279),#778,.F.);
#9419=ADVANCED_FACE('',(#1280),#779,.F.);
#9420=ADVANCED_FACE('',(#1281),#780,.F.);
#9421=ADVANCED_FACE('',(#1282),#781,.F.);
#9422=ADVANCED_FACE('',(#1283),#782,.F.);
#9423=ADVANCED_FACE('',(#1284),#783,.F.);
#9424=ADVANCED_FACE('',(#1285,#469),#784,.F.);
#9425=ADVANCED_FACE('',(#1286,#470),#785,.F.);
#9426=ADVANCED_FACE('',(#1287),#8959,.F.);
#9427=ADVANCED_FACE('',(#1288),#241,.T.);
#9428=ADVANCED_FACE('',(#1289),#126,.T.);
#9429=ADVANCED_FACE('',(#1290),#127,.F.);
#9430=ADVANCED_FACE('',(#1291),#242,.T.);
#9431=ADVANCED_FACE('',(#1292),#8960,.T.);
#9432=ADVANCED_FACE('',(#1293),#243,.F.);
#9433=ADVANCED_FACE('',(#1294),#244,.T.);
#9434=ADVANCED_FACE('',(#1295),#245,.T.);
#9435=ADVANCED_FACE('',(#1296),#128,.F.);
#9436=ADVANCED_FACE('',(#1297),#246,.F.);
#9437=ADVANCED_FACE('',(#1298),#247,.T.);
#9438=ADVANCED_FACE('',(#1299,#471),#786,.T.);
#9439=ADVANCED_FACE('',(#1300,#472),#787,.T.);
#9440=ADVANCED_FACE('',(#1301,#473),#788,.T.);
#9441=ADVANCED_FACE('',(#1302,#474),#789,.T.);
#9442=ADVANCED_FACE('',(#1303,#475),#790,.T.);
#9443=ADVANCED_FACE('',(#1304),#8961,.T.);
#9444=ADVANCED_FACE('',(#1305),#129,.F.);
#9445=ADVANCED_FACE('',(#1306),#8962,.F.);
#9446=ADVANCED_FACE('',(#1307),#130,.F.);
#9447=ADVANCED_FACE('',(#1308),#131,.T.);
#9448=ADVANCED_FACE('',(#1309,#476),#791,.F.);
#9449=ADVANCED_FACE('',(#1310),#132,.T.);
#9450=ADVANCED_FACE('',(#1311),#133,.T.);
#9451=ADVANCED_FACE('',(#1312),#134,.T.);
#9452=ADVANCED_FACE('',(#1313),#135,.T.);
#9453=ADVANCED_FACE('',(#1314),#136,.T.);
#9454=ADVANCED_FACE('',(#1315),#792,.F.);
#9455=ADVANCED_FACE('',(#1316),#793,.F.);
#9456=ADVANCED_FACE('',(#1317),#794,.F.);
#9457=ADVANCED_FACE('',(#1318),#795,.F.);
#9458=ADVANCED_FACE('',(#1319),#796,.F.);
#9459=ADVANCED_FACE('',(#1320),#797,.F.);
#9460=ADVANCED_FACE('',(#1321,#477),#798,.F.);
#9461=ADVANCED_FACE('',(#1322),#799,.F.);
#9462=ADVANCED_FACE('',(#1323),#800,.F.);
#9463=ADVANCED_FACE('',(#1324),#801,.F.);
#9464=ADVANCED_FACE('',(#1325),#802,.F.);
#9465=ADVANCED_FACE('',(#1326),#803,.F.);
#9466=ADVANCED_FACE('',(#1327),#804,.F.);
#9467=ADVANCED_FACE('',(#1328),#248,.T.);
#9468=ADVANCED_FACE('',(#1329),#137,.T.);
#9469=ADVANCED_FACE('',(#1330),#138,.T.);
#9470=ADVANCED_FACE('',(#1331),#8963,.T.);
#9471=ADVANCED_FACE('',(#1332),#249,.F.);
#9472=ADVANCED_FACE('',(#1333),#8964,.T.);
#9473=ADVANCED_FACE('',(#1334),#8965,.T.);
#9474=ADVANCED_FACE('',(#1335),#250,.F.);
#9475=ADVANCED_FACE('',(#1336),#8966,.T.);
#9476=ADVANCED_FACE('',(#1337),#139,.T.);
#9477=ADVANCED_FACE('',(#1338),#251,.F.);
#9478=ADVANCED_FACE('',(#1339),#8967,.T.);
#9479=ADVANCED_FACE('',(#1340),#140,.T.);
#9480=ADVANCED_FACE('',(#1341),#805,.T.);
#9481=ADVANCED_FACE('',(#1342),#806,.F.);
#9482=ADVANCED_FACE('',(#1343),#807,.F.);
#9483=ADVANCED_FACE('',(#1344,#478),#808,.F.);
#9484=ADVANCED_FACE('',(#1345,#479),#809,.F.);
#9485=ADVANCED_FACE('',(#1346,#480),#810,.F.);
#9486=ADVANCED_FACE('',(#1347),#811,.F.);
#9487=ADVANCED_FACE('',(#1348,#481),#812,.F.);
#9488=ADVANCED_FACE('',(#1349),#252,.T.);
#9489=ADVANCED_FACE('',(#1350),#253,.F.);
#9490=ADVANCED_FACE('',(#1351),#8968,.F.);
#9491=ADVANCED_FACE('',(#1352),#254,.T.);
#9492=ADVANCED_FACE('',(#1353),#141,.T.);
#9493=ADVANCED_FACE('',(#1354),#255,.F.);
#9494=ADVANCED_FACE('',(#1355),#256,.T.);
#9495=ADVANCED_FACE('',(#1356),#257,.F.);
#9496=ADVANCED_FACE('',(#1357),#258,.T.);
#9497=ADVANCED_FACE('',(#1358),#142,.F.);
#9498=ADVANCED_FACE('',(#1359),#259,.F.);
#9499=ADVANCED_FACE('',(#1360),#813,.F.);
#9500=ADVANCED_FACE('',(#1361),#814,.F.);
#9501=ADVANCED_FACE('',(#1362),#815,.F.);
#9502=ADVANCED_FACE('',(#1363),#816,.F.);
#9503=ADVANCED_FACE('',(#1364),#817,.F.);
#9504=ADVANCED_FACE('',(#1365),#818,.F.);
#9505=ADVANCED_FACE('',(#1366),#819,.F.);
#9506=ADVANCED_FACE('',(#1367),#820,.F.);
#9507=ADVANCED_FACE('',(#1368,#482),#821,.T.);
#9508=ADVANCED_FACE('',(#1369,#483),#822,.T.);
#9509=ADVANCED_FACE('',(#1370,#484),#823,.T.);
#9510=ADVANCED_FACE('',(#1371,#485),#824,.T.);
#9511=ADVANCED_FACE('',(#1372),#143,.T.);
#9512=ADVANCED_FACE('',(#1373),#144,.F.);
#9513=ADVANCED_FACE('',(#1374),#8969,.T.);
#9514=ADVANCED_FACE('',(#1375),#260,.T.);
#9515=ADVANCED_FACE('',(#1376),#8970,.T.);
#9516=ADVANCED_FACE('',(#1377),#261,.T.);
#9517=ADVANCED_FACE('',(#1378),#8971,.T.);
#9518=ADVANCED_FACE('',(#1379),#145,.F.);
#9519=ADVANCED_FACE('',(#1380),#146,.T.);
#9520=ADVANCED_FACE('',(#1381),#8972,.F.);
#9521=ADVANCED_FACE('',(#1382,#486),#825,.F.);
#9522=ADVANCED_FACE('',(#1383,#487),#826,.F.);
#9523=ADVANCED_FACE('',(#1384,#488),#827,.F.);
#9524=ADVANCED_FACE('',(#1385,#489),#828,.F.);
#9525=ADVANCED_FACE('',(#1386,#490),#829,.F.);
#9526=ADVANCED_FACE('',(#1387,#491),#830,.F.);
#9527=ADVANCED_FACE('',(#1388,#492),#831,.F.);
#9528=ADVANCED_FACE('',(#1389,#493),#832,.F.);
#9529=ADVANCED_FACE('',(#1390),#8973,.F.);
#9530=ADVANCED_FACE('',(#1391),#262,.F.);
#9531=ADVANCED_FACE('',(#1392),#8974,.F.);
#9532=ADVANCED_FACE('',(#1393),#263,.F.);
#9533=ADVANCED_FACE('',(#1394),#8975,.F.);
#9534=ADVANCED_FACE('',(#1395),#264,.F.);
#9535=ADVANCED_FACE('',(#1396),#147,.T.);
#9536=ADVANCED_FACE('',(#1397),#265,.T.);
#9537=ADVANCED_FACE('',(#1398),#148,.T.);
#9538=ADVANCED_FACE('',(#1399),#149,.T.);
#9539=ADVANCED_FACE('',(#1400),#266,.T.);
#9540=ADVANCED_FACE('',(#1401),#150,.T.);
#9541=ADVANCED_FACE('',(#1402),#267,.F.);
#9542=ADVANCED_FACE('',(#1403,#494),#833,.T.);
#9543=ADVANCED_FACE('',(#1404,#495),#834,.T.);
#9544=ADVANCED_FACE('',(#1405,#496),#835,.T.);
#9545=ADVANCED_FACE('',(#1406,#497),#836,.T.);
#9546=ADVANCED_FACE('',(#1407),#8976,.F.);
#9547=ADVANCED_FACE('',(#1408),#8977,.T.);
#9548=ADVANCED_FACE('',(#1409,#498),#837,.T.);
#9549=ADVANCED_FACE('',(#1410,#499),#838,.T.);
#9550=ADVANCED_FACE('',(#1411),#151,.F.);
#9551=ADVANCED_FACE('',(#1412),#8978,.F.);
#9552=ADVANCED_FACE('',(#1413),#152,.F.);
#9553=ADVANCED_FACE('',(#1414),#8979,.T.);
#9554=ADVANCED_FACE('',(#1415,#500),#839,.T.);
#9555=ADVANCED_FACE('',(#1416,#501),#840,.T.);
#9556=CLOSED_SHELL('',(#8980,#8981,#8982,#8983,#8984,#8985,#8986,#8987,
#8988,#8989,#8990,#8991,#8992,#8993,#8994,#8995,#8996,#8997,#8998,#8999,
#9000,#9001,#9002,#9003,#9004,#9005,#9006,#9007,#9008,#9009,#9010,#9011,
#9012,#9013,#9014,#9015,#9016,#9017,#9018,#9019,#9020,#9021,#9022,#9023,
#9024,#9025,#9026,#9027,#9028,#9029,#9030,#9031,#9032,#9033,#9034,#9035,
#9036,#9037,#9038,#9039,#9040,#9041,#9042,#9043,#9044,#9045,#9046,#9047,
#9048,#9049,#9050,#9051,#9052,#9053,#9054,#9055,#9056,#9057,#9058,#9059,
#9060));
#9557=CLOSED_SHELL('',(#9061,#9062,#9063,#9064,#9065,#9066,#9067,#9068,
#9069,#9070,#9071,#9072,#9073,#9074,#9075,#9076,#9077,#9078,#9079,#9080,
#9081,#9082,#9083,#9084,#9085,#9086,#9087,#9088,#9089,#9090,#9091,#9092,
#9093,#9094,#9095,#9096,#9097,#9098,#9099,#9100,#9101,#9102,#9103,#9104,
#9105,#9106,#9107,#9108,#9109,#9110,#9111,#9112,#9113,#9114,#9115,#9116,
#9117,#9118,#9119,#9120,#9121,#9122,#9123,#9124,#9125,#9126,#9127,#9128,
#9129,#9130,#9131,#9132,#9133,#9134,#9135,#9136,#9137,#9138));
#9558=CLOSED_SHELL('',(#9139,#9140,#9141,#9142,#9143,#9144,#9145,#9146,
#9147,#9148,#9149,#9150,#9151,#9152,#9153,#9154,#9155,#9156,#9157,#9158,
#9159,#9160,#9161,#9162,#9163,#9164,#9165,#9166,#9167,#9168,#9169,#9170,
#9171,#9172,#9173,#9174,#9175,#9176));
#9559=CLOSED_SHELL('',(#9177,#9178,#9179,#9180,#9181,#9182,#9183,#9184,
#9185,#9186,#9187,#9188,#9189,#9190,#9191,#9192,#9193,#9194,#9195,#9196,
#9197,#9198,#9199,#9200,#9201,#9202,#9203,#9204,#9205,#9206,#9207,#9208,
#9209,#9210,#9211,#9212,#9213,#9214));
#9560=CLOSED_SHELL('',(#9215,#9216,#9217,#9218,#9219,#9220,#9221,#9222,
#9223,#9224,#9225,#9226,#9227,#9228,#9229,#9230,#9231,#9232,#9233,#9234,
#9235,#9236,#9237,#9238,#9239,#9240,#9241,#9242,#9243,#9244,#9245,#9246,
#9247,#9248,#9249,#9250,#9251,#9252,#9253,#9254,#9255));
#9561=CLOSED_SHELL('',(#9256,#9257,#9258,#9259,#9260,#9261,#9262,#9263,
#9264,#9265,#9266,#9267,#9268,#9269,#9270,#9271,#9272,#9273,#9274,#9275,
#9276,#9277));
#9562=CLOSED_SHELL('',(#9278,#9279,#9280,#9281,#9282,#9283,#9284,#9285,
#9286,#9287,#9288,#9289,#9290,#9291,#9292,#9293,#9294,#9295,#9296,#9297,
#9298,#9299,#9300,#9301,#9302,#9303,#9304,#9305,#9306,#9307,#9308,#9309,
#9310,#9311,#9312,#9313,#9314,#9315,#9316,#9317,#9318,#9319,#9320,#9321,
#9322,#9323,#9324,#9325,#9326,#9327,#9328,#9329,#9330,#9331,#9332,#9333,
#9334,#9335,#9336,#9337,#9338,#9339,#9340,#9341,#9342,#9343,#9344,#9345,
#9346,#9347,#9348,#9349,#9350,#9351,#9352,#9353,#9354,#9355,#9356,#9357,
#9358,#9359,#9360,#9361,#9362,#9363,#9364,#9365,#9366,#9367,#9368,#9369,
#9370,#9371,#9372,#9373,#9374,#9375,#9376,#9377,#9378,#9379,#9380,#9381,
#9382,#9383,#9384,#9385,#9386,#9387,#9388,#9389,#9390,#9391,#9392,#9393,
#9394,#9395,#9396,#9397,#9398,#9399,#9400,#9401,#9402,#9403,#9404));
#9563=CLOSED_SHELL('',(#9405,#9406,#9407,#9408,#9409,#9410,#9411,#9412,
#9413,#9414,#9415,#9416,#9417,#9418,#9419,#9420,#9421,#9422,#9423,#9424,
#9425));
#9564=CLOSED_SHELL('',(#9426,#9427,#9428,#9429,#9430,#9431,#9432,#9433,
#9434,#9435,#9436,#9437,#9438,#9439,#9440,#9441,#9442));
#9565=CLOSED_SHELL('',(#9443,#9444,#9445,#9446,#9447,#9448,#9449,#9450,
#9451,#9452,#9453,#9454,#9455,#9456,#9457,#9458,#9459,#9460,#9461,#9462,
#9463,#9464,#9465,#9466));
#9566=CLOSED_SHELL('',(#9467,#9468,#9469,#9470,#9471,#9472,#9473,#9474,
#9475,#9476,#9477,#9478,#9479,#9480,#9481,#9482,#9483,#9484,#9485,#9486,
#9487));
#9567=CLOSED_SHELL('',(#9488,#9489,#9490,#9491,#9492,#9493,#9494,#9495,
#9496,#9497,#9498,#9499,#9500,#9501,#9502,#9503,#9504,#9505,#9506,#9507,
#9508,#9509,#9510));
#9568=CLOSED_SHELL('',(#9511,#9512,#9513,#9514,#9515,#9516,#9517,#9518,
#9519,#9520,#9521,#9522,#9523,#9524,#9525,#9526,#9527,#9528));
#9569=CLOSED_SHELL('',(#9529,#9530,#9531,#9532,#9533,#9534,#9535,#9536,
#9537,#9538,#9539,#9540,#9541,#9542,#9543,#9544,#9545));
#9570=CLOSED_SHELL('',(#9546,#9547,#9548,#9549));
#9571=CLOSED_SHELL('',(#9550,#9551,#9552,#9553,#9554,#9555));
#9572=DERIVED_UNIT_ELEMENT(#9604,1.);
#9573=DERIVED_UNIT_ELEMENT(#18008,-3.);
#9574=DERIVED_UNIT_ELEMENT(#9604,1.);
#9575=DERIVED_UNIT_ELEMENT(#18008,-3.);
#9576=DERIVED_UNIT_ELEMENT(#9604,1.);
#9577=DERIVED_UNIT_ELEMENT(#18008,-3.);
#9578=DERIVED_UNIT_ELEMENT(#9604,1.);
#9579=DERIVED_UNIT_ELEMENT(#18008,-3.);
#9580=DERIVED_UNIT_ELEMENT(#9604,1.);
#9581=DERIVED_UNIT_ELEMENT(#18008,-3.);
#9582=DERIVED_UNIT_ELEMENT(#9604,1.);
#9583=DERIVED_UNIT_ELEMENT(#18008,-3.);
#9584=DERIVED_UNIT_ELEMENT(#9604,1.);
#9585=DERIVED_UNIT_ELEMENT(#18008,-3.);
#9586=DERIVED_UNIT_ELEMENT(#9604,1.);
#9587=DERIVED_UNIT_ELEMENT(#18008,-3.);
#9588=DERIVED_UNIT_ELEMENT(#9604,1.);
#9589=DERIVED_UNIT_ELEMENT(#18008,-3.);
#9590=DERIVED_UNIT_ELEMENT(#9604,1.);
#9591=DERIVED_UNIT_ELEMENT(#18008,-3.);
#9592=DERIVED_UNIT_ELEMENT(#9604,1.);
#9593=DERIVED_UNIT_ELEMENT(#18008,-3.);
#9594=DERIVED_UNIT_ELEMENT(#9604,1.);
#9595=DERIVED_UNIT_ELEMENT(#18008,-3.);
#9596=DERIVED_UNIT_ELEMENT(#9604,1.);
#9597=DERIVED_UNIT_ELEMENT(#18008,-3.);
#9598=DERIVED_UNIT_ELEMENT(#9604,1.);
#9599=DERIVED_UNIT_ELEMENT(#18008,-3.);
#9600=DERIVED_UNIT_ELEMENT(#9604,1.);
#9601=DERIVED_UNIT_ELEMENT(#18008,-3.);
#9602=DERIVED_UNIT_ELEMENT(#9604,1.);
#9603=DERIVED_UNIT_ELEMENT(#18008,-3.);
#9604=(
MASS_UNIT()
NAMED_UNIT(*)
SI_UNIT(.KILO.,.GRAM.)
);
#9605=DERIVED_UNIT((#9572,#9573));
#9606=DERIVED_UNIT((#9574,#9575));
#9607=DERIVED_UNIT((#9576,#9577));
#9608=DERIVED_UNIT((#9578,#9579));
#9609=DERIVED_UNIT((#9580,#9581));
#9610=DERIVED_UNIT((#9582,#9583));
#9611=DERIVED_UNIT((#9584,#9585));
#9612=DERIVED_UNIT((#9586,#9587));
#9613=DERIVED_UNIT((#9588,#9589));
#9614=DERIVED_UNIT((#9590,#9591));
#9615=DERIVED_UNIT((#9592,#9593));
#9616=DERIVED_UNIT((#9594,#9595));
#9617=DERIVED_UNIT((#9596,#9597));
#9618=DERIVED_UNIT((#9598,#9599));
#9619=DERIVED_UNIT((#9600,#9601));
#9620=DERIVED_UNIT((#9602,#9603));
#9621=MEASURE_REPRESENTATION_ITEM('density measure',
POSITIVE_RATIO_MEASURE(7850.),#9605);
#9622=MEASURE_REPRESENTATION_ITEM('density measure',
POSITIVE_RATIO_MEASURE(7850.),#9606);
#9623=MEASURE_REPRESENTATION_ITEM('density measure',
POSITIVE_RATIO_MEASURE(7850.),#9607);
#9624=MEASURE_REPRESENTATION_ITEM('density measure',
POSITIVE_RATIO_MEASURE(7850.),#9608);
#9625=MEASURE_REPRESENTATION_ITEM('density measure',
POSITIVE_RATIO_MEASURE(7850.),#9609);
#9626=MEASURE_REPRESENTATION_ITEM('density measure',
POSITIVE_RATIO_MEASURE(7850.),#9610);
#9627=MEASURE_REPRESENTATION_ITEM('density measure',
POSITIVE_RATIO_MEASURE(7850.),#9611);
#9628=MEASURE_REPRESENTATION_ITEM('density measure',
POSITIVE_RATIO_MEASURE(7850.),#9612);
#9629=MEASURE_REPRESENTATION_ITEM('density measure',
POSITIVE_RATIO_MEASURE(7850.),#9613);
#9630=MEASURE_REPRESENTATION_ITEM('density measure',
POSITIVE_RATIO_MEASURE(7850.),#9614);
#9631=MEASURE_REPRESENTATION_ITEM('density measure',
POSITIVE_RATIO_MEASURE(7850.),#9615);
#9632=MEASURE_REPRESENTATION_ITEM('density measure',
POSITIVE_RATIO_MEASURE(7850.),#9616);
#9633=MEASURE_REPRESENTATION_ITEM('density measure',
POSITIVE_RATIO_MEASURE(7850.),#9617);
#9634=MEASURE_REPRESENTATION_ITEM('density measure',
POSITIVE_RATIO_MEASURE(7850.),#9618);
#9635=MEASURE_REPRESENTATION_ITEM('density measure',
POSITIVE_RATIO_MEASURE(7850.),#9619);
#9636=MEASURE_REPRESENTATION_ITEM('density measure',
POSITIVE_RATIO_MEASURE(7850.),#9620);
#9637=PROPERTY_DEFINITION_REPRESENTATION(#9717,#9669);
#9638=PROPERTY_DEFINITION_REPRESENTATION(#9718,#9670);
#9639=PROPERTY_DEFINITION_REPRESENTATION(#9719,#9671);
#9640=PROPERTY_DEFINITION_REPRESENTATION(#9720,#9672);
#9641=PROPERTY_DEFINITION_REPRESENTATION(#9721,#9673);
#9642=PROPERTY_DEFINITION_REPRESENTATION(#9722,#9674);
#9643=PROPERTY_DEFINITION_REPRESENTATION(#9723,#9675);
#9644=PROPERTY_DEFINITION_REPRESENTATION(#9724,#9676);
#9645=PROPERTY_DEFINITION_REPRESENTATION(#9725,#9677);
#9646=PROPERTY_DEFINITION_REPRESENTATION(#9726,#9678);
#9647=PROPERTY_DEFINITION_REPRESENTATION(#9727,#9679);
#9648=PROPERTY_DEFINITION_REPRESENTATION(#9728,#9680);
#9649=PROPERTY_DEFINITION_REPRESENTATION(#9729,#9681);
#9650=PROPERTY_DEFINITION_REPRESENTATION(#9730,#9682);
#9651=PROPERTY_DEFINITION_REPRESENTATION(#9731,#9683);
#9652=PROPERTY_DEFINITION_REPRESENTATION(#9732,#9684);
#9653=PROPERTY_DEFINITION_REPRESENTATION(#9733,#9685);
#9654=PROPERTY_DEFINITION_REPRESENTATION(#9734,#9686);
#9655=PROPERTY_DEFINITION_REPRESENTATION(#9735,#9687);
#9656=PROPERTY_DEFINITION_REPRESENTATION(#9736,#9688);
#9657=PROPERTY_DEFINITION_REPRESENTATION(#9737,#9689);
#9658=PROPERTY_DEFINITION_REPRESENTATION(#9738,#9690);
#9659=PROPERTY_DEFINITION_REPRESENTATION(#9739,#9691);
#9660=PROPERTY_DEFINITION_REPRESENTATION(#9740,#9692);
#9661=PROPERTY_DEFINITION_REPRESENTATION(#9741,#9693);
#9662=PROPERTY_DEFINITION_REPRESENTATION(#9742,#9694);
#9663=PROPERTY_DEFINITION_REPRESENTATION(#9743,#9695);
#9664=PROPERTY_DEFINITION_REPRESENTATION(#9744,#9696);
#9665=PROPERTY_DEFINITION_REPRESENTATION(#9745,#9697);
#9666=PROPERTY_DEFINITION_REPRESENTATION(#9746,#9698);
#9667=PROPERTY_DEFINITION_REPRESENTATION(#9747,#9699);
#9668=PROPERTY_DEFINITION_REPRESENTATION(#9748,#9700);
#9669=REPRESENTATION('material name',(#9701),#17988);
#9670=REPRESENTATION('density',(#9621),#17988);
#9671=REPRESENTATION('material name',(#9702),#17989);
#9672=REPRESENTATION('density',(#9622),#17989);
#9673=REPRESENTATION('material name',(#9703),#17990);
#9674=REPRESENTATION('density',(#9623),#17990);
#9675=REPRESENTATION('material name',(#9704),#17991);
#9676=REPRESENTATION('density',(#9624),#17991);
#9677=REPRESENTATION('material name',(#9705),#17992);
#9678=REPRESENTATION('density',(#9625),#17992);
#9679=REPRESENTATION('material name',(#9706),#17993);
#9680=REPRESENTATION('density',(#9626),#17993);
#9681=REPRESENTATION('material name',(#9707),#17996);
#9682=REPRESENTATION('density',(#9627),#17996);
#9683=REPRESENTATION('material name',(#9708),#17997);
#9684=REPRESENTATION('density',(#9628),#17997);
#9685=REPRESENTATION('material name',(#9709),#17998);
#9686=REPRESENTATION('density',(#9629),#17998);
#9687=REPRESENTATION('material name',(#9710),#17999);
#9688=REPRESENTATION('density',(#9630),#17999);
#9689=REPRESENTATION('material name',(#9711),#18000);
#9690=REPRESENTATION('density',(#9631),#18000);
#9691=REPRESENTATION('material name',(#9712),#18001);
#9692=REPRESENTATION('density',(#9632),#18001);
#9693=REPRESENTATION('material name',(#9713),#18002);
#9694=REPRESENTATION('density',(#9633),#18002);
#9695=REPRESENTATION('material name',(#9714),#18003);
#9696=REPRESENTATION('density',(#9634),#18003);
#9697=REPRESENTATION('material name',(#9715),#18004);
#9698=REPRESENTATION('density',(#9635),#18004);
#9699=REPRESENTATION('material name',(#9716),#18005);
#9700=REPRESENTATION('density',(#9636),#18005);
#9701=DESCRIPTIVE_REPRESENTATION_ITEM('Steel','Steel');
#9702=DESCRIPTIVE_REPRESENTATION_ITEM('Steel','Steel');
#9703=DESCRIPTIVE_REPRESENTATION_ITEM('Steel','Steel');
#9704=DESCRIPTIVE_REPRESENTATION_ITEM('Steel','Steel');
#9705=DESCRIPTIVE_REPRESENTATION_ITEM('Steel','Steel');
#9706=DESCRIPTIVE_REPRESENTATION_ITEM('Steel','Steel');
#9707=DESCRIPTIVE_REPRESENTATION_ITEM('Steel','Steel');
#9708=DESCRIPTIVE_REPRESENTATION_ITEM('Steel','Steel');
#9709=DESCRIPTIVE_REPRESENTATION_ITEM('Steel','Steel');
#9710=DESCRIPTIVE_REPRESENTATION_ITEM('Steel','Steel');
#9711=DESCRIPTIVE_REPRESENTATION_ITEM('Steel','Steel');
#9712=DESCRIPTIVE_REPRESENTATION_ITEM('Steel','Steel');
#9713=DESCRIPTIVE_REPRESENTATION_ITEM('Steel','Steel');
#9714=DESCRIPTIVE_REPRESENTATION_ITEM('Steel','Steel');
#9715=DESCRIPTIVE_REPRESENTATION_ITEM('Steel','Steel');
#9716=DESCRIPTIVE_REPRESENTATION_ITEM('Steel','Steel');
#9717=PROPERTY_DEFINITION('material property','material name',#18091);
#9718=PROPERTY_DEFINITION('material property','density of part',#18091);
#9719=PROPERTY_DEFINITION('material property','material name',#18092);
#9720=PROPERTY_DEFINITION('material property','density of part',#18092);
#9721=PROPERTY_DEFINITION('material property','material name',#18093);
#9722=PROPERTY_DEFINITION('material property','density of part',#18093);
#9723=PROPERTY_DEFINITION('material property','material name',#18094);
#9724=PROPERTY_DEFINITION('material property','density of part',#18094);
#9725=PROPERTY_DEFINITION('material property','material name',#18095);
#9726=PROPERTY_DEFINITION('material property','density of part',#18095);
#9727=PROPERTY_DEFINITION('material property','material name',#18096);
#9728=PROPERTY_DEFINITION('material property','density of part',#18096);
#9729=PROPERTY_DEFINITION('material property','material name',#18099);
#9730=PROPERTY_DEFINITION('material property','density of part',#18099);
#9731=PROPERTY_DEFINITION('material property','material name',#18100);
#9732=PROPERTY_DEFINITION('material property','density of part',#18100);
#9733=PROPERTY_DEFINITION('material property','material name',#18101);
#9734=PROPERTY_DEFINITION('material property','density of part',#18101);
#9735=PROPERTY_DEFINITION('material property','material name',#18102);
#9736=PROPERTY_DEFINITION('material property','density of part',#18102);
#9737=PROPERTY_DEFINITION('material property','material name',#18103);
#9738=PROPERTY_DEFINITION('material property','density of part',#18103);
#9739=PROPERTY_DEFINITION('material property','material name',#18104);
#9740=PROPERTY_DEFINITION('material property','density of part',#18104);
#9741=PROPERTY_DEFINITION('material property','material name',#18105);
#9742=PROPERTY_DEFINITION('material property','density of part',#18105);
#9743=PROPERTY_DEFINITION('material property','material name',#18106);
#9744=PROPERTY_DEFINITION('material property','density of part',#18106);
#9745=PROPERTY_DEFINITION('material property','material name',#18107);
#9746=PROPERTY_DEFINITION('material property','density of part',#18107);
#9747=PROPERTY_DEFINITION('material property','material name',#18108);
#9748=PROPERTY_DEFINITION('material property','density of part',#18108);
#9749=AXIS2_PLACEMENT_3D('',#13809,#10861,#10862);
#9750=AXIS2_PLACEMENT_3D('',#13810,#10863,#10864);
#9751=AXIS2_PLACEMENT_3D('',#13811,#10865,#10866);
#9752=AXIS2_PLACEMENT_3D('',#13813,#10867,#10868);
#9753=AXIS2_PLACEMENT_3D('',#13816,#10870,#10871);
#9754=AXIS2_PLACEMENT_3D('',#13817,#10872,#10873);
#9755=AXIS2_PLACEMENT_3D('',#13819,#10874,#10875);
#9756=AXIS2_PLACEMENT_3D('',#13822,#10877,#10878);
#9757=AXIS2_PLACEMENT_3D('',#13823,#10879,#10880);
#9758=AXIS2_PLACEMENT_3D('',#13825,#10881,#10882);
#9759=AXIS2_PLACEMENT_3D('',#13828,#10884,#10885);
#9760=AXIS2_PLACEMENT_3D('',#13829,#10886,#10887);
#9761=AXIS2_PLACEMENT_3D('',#13831,#10888,#10889);
#9762=AXIS2_PLACEMENT_3D('',#13834,#10891,#10892);
#9763=AXIS2_PLACEMENT_3D('',#13835,#10893,#10894);
#9764=AXIS2_PLACEMENT_3D('',#13837,#10895,#10896);
#9765=AXIS2_PLACEMENT_3D('',#13840,#10898,#10899);
#9766=AXIS2_PLACEMENT_3D('',#13841,#10900,#10901);
#9767=AXIS2_PLACEMENT_3D('',#13843,#10902,#10903);
#9768=AXIS2_PLACEMENT_3D('',#13846,#10905,#10906);
#9769=AXIS2_PLACEMENT_3D('',#13847,#10907,#10908);
#9770=AXIS2_PLACEMENT_3D('',#13849,#10909,#10910);
#9771=AXIS2_PLACEMENT_3D('',#13852,#10912,#10913);
#9772=AXIS2_PLACEMENT_3D('',#13853,#10914,#10915);
#9773=AXIS2_PLACEMENT_3D('',#13855,#10916,#10917);
#9774=AXIS2_PLACEMENT_3D('',#13858,#10919,#10920);
#9775=AXIS2_PLACEMENT_3D('',#13859,#10921,#10922);
#9776=AXIS2_PLACEMENT_3D('',#13861,#10923,#10924);
#9777=AXIS2_PLACEMENT_3D('',#13864,#10926,#10927);
#9778=AXIS2_PLACEMENT_3D('',#13865,#10928,#10929);
#9779=AXIS2_PLACEMENT_3D('',#13867,#10930,#10931);
#9780=AXIS2_PLACEMENT_3D('',#13870,#10933,#10934);
#9781=AXIS2_PLACEMENT_3D('',#13871,#10935,#10936);
#9782=AXIS2_PLACEMENT_3D('',#13873,#10937,#10938);
#9783=AXIS2_PLACEMENT_3D('',#13876,#10940,#10941);
#9784=AXIS2_PLACEMENT_3D('',#13877,#10942,#10943);
#9785=AXIS2_PLACEMENT_3D('',#13882,#10945,#10946);
#9786=AXIS2_PLACEMENT_3D('',#13886,#10949,#10950);
#9787=AXIS2_PLACEMENT_3D('',#13891,#10952,#10953);
#9788=AXIS2_PLACEMENT_3D('',#13895,#10956,#10957);
#9789=AXIS2_PLACEMENT_3D('',#13902,#10962,#10963);
#9790=AXIS2_PLACEMENT_3D('',#13911,#10968,#10969);
#9791=AXIS2_PLACEMENT_3D('',#13915,#10971,#10972);
#9792=AXIS2_PLACEMENT_3D('',#13919,#10975,#10976);
#9793=AXIS2_PLACEMENT_3D('',#13923,#10978,#10979);
#9794=AXIS2_PLACEMENT_3D('',#13927,#10982,#10983);
#9795=AXIS2_PLACEMENT_3D('',#13932,#10985,#10986);
#9796=AXIS2_PLACEMENT_3D('',#13935,#10988,#10989);
#9797=AXIS2_PLACEMENT_3D('',#13936,#10990,#10991);
#9798=AXIS2_PLACEMENT_3D('',#13942,#10995,#10996);
#9799=AXIS2_PLACEMENT_3D('',#13947,#10998,#10999);
#9800=AXIS2_PLACEMENT_3D('',#13950,#11001,#11002);
#9801=AXIS2_PLACEMENT_3D('',#13951,#11003,#11004);
#9802=AXIS2_PLACEMENT_3D('',#13957,#11008,#11009);
#9803=AXIS2_PLACEMENT_3D('',#13961,#11011,#11012);
#9804=AXIS2_PLACEMENT_3D('',#13962,#11013,#11014);
#9805=AXIS2_PLACEMENT_3D('',#13963,#11015,#11016);
#9806=AXIS2_PLACEMENT_3D('',#13969,#11020,#11021);
#9807=AXIS2_PLACEMENT_3D('',#13974,#11023,#11024);
#9808=AXIS2_PLACEMENT_3D('',#13977,#11026,#11027);
#9809=AXIS2_PLACEMENT_3D('',#13978,#11028,#11029);
#9810=AXIS2_PLACEMENT_3D('',#13981,#11032,#11033);
#9811=AXIS2_PLACEMENT_3D('',#13982,#11034,#11035);
#9812=AXIS2_PLACEMENT_3D('',#13983,#11036,#11037);
#9813=AXIS2_PLACEMENT_3D('',#13984,#11038,#11039);
#9814=AXIS2_PLACEMENT_3D('',#13988,#11041,#11042);
#9815=AXIS2_PLACEMENT_3D('',#13989,#11043,#11044);
#9816=AXIS2_PLACEMENT_3D('',#13990,#11045,#11046);
#9817=AXIS2_PLACEMENT_3D('',#13993,#11049,#11050);
#9818=AXIS2_PLACEMENT_3D('',#13997,#11052,#11053);
#9819=AXIS2_PLACEMENT_3D('',#13998,#11054,#11055);
#9820=AXIS2_PLACEMENT_3D('',#13999,#11056,#11057);
#9821=AXIS2_PLACEMENT_3D('',#14005,#11061,#11062);
#9822=AXIS2_PLACEMENT_3D('',#14007,#11063,#11064);
#9823=AXIS2_PLACEMENT_3D('',#14010,#11066,#11067);
#9824=AXIS2_PLACEMENT_3D('',#14011,#11068,#11069);
#9825=AXIS2_PLACEMENT_3D('',#14015,#11071,#11072);
#9826=AXIS2_PLACEMENT_3D('',#14016,#11073,#11074);
#9827=AXIS2_PLACEMENT_3D('',#14017,#11075,#11076);
#9828=AXIS2_PLACEMENT_3D('',#14023,#11080,#11081);
#9829=AXIS2_PLACEMENT_3D('',#14028,#11083,#11084);
#9830=AXIS2_PLACEMENT_3D('',#14031,#11086,#11087);
#9831=AXIS2_PLACEMENT_3D('',#14032,#11088,#11089);
#9832=AXIS2_PLACEMENT_3D('',#14035,#11092,#11093);
#9833=AXIS2_PLACEMENT_3D('',#14040,#11097,#11098);
#9834=AXIS2_PLACEMENT_3D('',#14044,#11101,#11102);
#9835=AXIS2_PLACEMENT_3D('',#14047,#11105,#11106);
#9836=AXIS2_PLACEMENT_3D('',#14049,#11108,#11109);
#9837=AXIS2_PLACEMENT_3D('',#14051,#11111,#11112);
#9838=AXIS2_PLACEMENT_3D('',#14052,#11113,#11114);
#9839=AXIS2_PLACEMENT_3D('',#14054,#11116,#11117);
#9840=AXIS2_PLACEMENT_3D('',#14056,#11119,#11120);
#9841=AXIS2_PLACEMENT_3D('',#14058,#11122,#11123);
#9842=AXIS2_PLACEMENT_3D('',#14060,#11125,#11126);
#9843=AXIS2_PLACEMENT_3D('',#14062,#11128,#11129);
#9844=AXIS2_PLACEMENT_3D('',#14066,#11132,#11133);
#9845=AXIS2_PLACEMENT_3D('',#14070,#11136,#11137);
#9846=AXIS2_PLACEMENT_3D('',#14073,#11140,#11141);
#9847=AXIS2_PLACEMENT_3D('',#14075,#11143,#11144);
#9848=AXIS2_PLACEMENT_3D('',#14077,#11146,#11147);
#9849=AXIS2_PLACEMENT_3D('',#14079,#11149,#11150);
#9850=AXIS2_PLACEMENT_3D('',#14081,#11152,#11153);
#9851=AXIS2_PLACEMENT_3D('',#14084,#11156,#11157);
#9852=AXIS2_PLACEMENT_3D('',#14088,#11161,#11162);
#9853=AXIS2_PLACEMENT_3D('',#14090,#11164,#11165);
#9854=AXIS2_PLACEMENT_3D('',#14091,#11166,#11167);
#9855=AXIS2_PLACEMENT_3D('',#14092,#11168,#11169);
#9856=AXIS2_PLACEMENT_3D('',#14093,#11170,#11171);
#9857=AXIS2_PLACEMENT_3D('',#14095,#11172,#11173);
#9858=AXIS2_PLACEMENT_3D('',#14098,#11175,#11176);
#9859=AXIS2_PLACEMENT_3D('',#14099,#11177,#11178);
#9860=AXIS2_PLACEMENT_3D('',#14101,#11179,#11180);
#9861=AXIS2_PLACEMENT_3D('',#14103,#11181,#11182);
#9862=AXIS2_PLACEMENT_3D('',#14105,#11184,#11185);
#9863=AXIS2_PLACEMENT_3D('',#14107,#11187,#11188);
#9864=AXIS2_PLACEMENT_3D('',#14109,#11190,#11191);
#9865=AXIS2_PLACEMENT_3D('',#14115,#11195,#11196);
#9866=AXIS2_PLACEMENT_3D('',#14121,#11200,#11201);
#9867=AXIS2_PLACEMENT_3D('',#14127,#11205,#11206);
#9868=AXIS2_PLACEMENT_3D('',#14133,#11210,#11211);
#9869=AXIS2_PLACEMENT_3D('',#14135,#11213,#11214);
#9870=AXIS2_PLACEMENT_3D('',#14137,#11216,#11217);
#9871=AXIS2_PLACEMENT_3D('',#14138,#11218,#11219);
#9872=AXIS2_PLACEMENT_3D('',#14140,#11220,#11221);
#9873=AXIS2_PLACEMENT_3D('',#14142,#11222,#11223);
#9874=AXIS2_PLACEMENT_3D('',#14144,#11225,#11226);
#9875=AXIS2_PLACEMENT_3D('',#14146,#11227,#11228);
#9876=AXIS2_PLACEMENT_3D('',#14148,#11229,#11230);
#9877=AXIS2_PLACEMENT_3D('',#14150,#11232,#11233);
#9878=AXIS2_PLACEMENT_3D('',#14152,#11235,#11236);
#9879=AXIS2_PLACEMENT_3D('',#14154,#11238,#11239);
#9880=AXIS2_PLACEMENT_3D('',#14160,#11243,#11244);
#9881=AXIS2_PLACEMENT_3D('',#14166,#11248,#11249);
#9882=AXIS2_PLACEMENT_3D('',#14172,#11253,#11254);
#9883=AXIS2_PLACEMENT_3D('',#14178,#11258,#11259);
#9884=AXIS2_PLACEMENT_3D('',#14180,#11261,#11262);
#9885=AXIS2_PLACEMENT_3D('',#14182,#11264,#11265);
#9886=AXIS2_PLACEMENT_3D('',#14183,#11266,#11267);
#9887=AXIS2_PLACEMENT_3D('',#14184,#11268,#11269);
#9888=AXIS2_PLACEMENT_3D('',#14186,#11270,#11271);
#9889=AXIS2_PLACEMENT_3D('',#14189,#11273,#11274);
#9890=AXIS2_PLACEMENT_3D('',#14190,#11275,#11276);
#9891=AXIS2_PLACEMENT_3D('',#14192,#11277,#11278);
#9892=AXIS2_PLACEMENT_3D('',#14195,#11280,#11281);
#9893=AXIS2_PLACEMENT_3D('',#14196,#11282,#11283);
#9894=AXIS2_PLACEMENT_3D('',#14198,#11284,#11285);
#9895=AXIS2_PLACEMENT_3D('',#14201,#11287,#11288);
#9896=AXIS2_PLACEMENT_3D('',#14202,#11289,#11290);
#9897=AXIS2_PLACEMENT_3D('',#14204,#11291,#11292);
#9898=AXIS2_PLACEMENT_3D('',#14207,#11294,#11295);
#9899=AXIS2_PLACEMENT_3D('',#14208,#11296,#11297);
#9900=AXIS2_PLACEMENT_3D('',#14210,#11298,#11299);
#9901=AXIS2_PLACEMENT_3D('',#14213,#11301,#11302);
#9902=AXIS2_PLACEMENT_3D('',#14214,#11303,#11304);
#9903=AXIS2_PLACEMENT_3D('',#14216,#11305,#11306);
#9904=AXIS2_PLACEMENT_3D('',#14219,#11308,#11309);
#9905=AXIS2_PLACEMENT_3D('',#14220,#11310,#11311);
#9906=AXIS2_PLACEMENT_3D('',#14222,#11312,#11313);
#9907=AXIS2_PLACEMENT_3D('',#14225,#11315,#11316);
#9908=AXIS2_PLACEMENT_3D('',#14226,#11317,#11318);
#9909=AXIS2_PLACEMENT_3D('',#14228,#11319,#11320);
#9910=AXIS2_PLACEMENT_3D('',#14231,#11322,#11323);
#9911=AXIS2_PLACEMENT_3D('',#14232,#11324,#11325);
#9912=AXIS2_PLACEMENT_3D('',#14237,#11327,#11328);
#9913=AXIS2_PLACEMENT_3D('',#14241,#11331,#11332);
#9914=AXIS2_PLACEMENT_3D('',#14246,#11334,#11335);
#9915=AXIS2_PLACEMENT_3D('',#14250,#11338,#11339);
#9916=AXIS2_PLACEMENT_3D('',#14257,#11344,#11345);
#9917=AXIS2_PLACEMENT_3D('',#14266,#11350,#11351);
#9918=AXIS2_PLACEMENT_3D('',#14270,#11353,#11354);
#9919=AXIS2_PLACEMENT_3D('',#14274,#11357,#11358);
#9920=AXIS2_PLACEMENT_3D('',#14278,#11360,#11361);
#9921=AXIS2_PLACEMENT_3D('',#14282,#11364,#11365);
#9922=AXIS2_PLACEMENT_3D('',#14287,#11367,#11368);
#9923=AXIS2_PLACEMENT_3D('',#14290,#11370,#11371);
#9924=AXIS2_PLACEMENT_3D('',#14291,#11372,#11373);
#9925=AXIS2_PLACEMENT_3D('',#14297,#11377,#11378);
#9926=AXIS2_PLACEMENT_3D('',#14302,#11380,#11381);
#9927=AXIS2_PLACEMENT_3D('',#14305,#11383,#11384);
#9928=AXIS2_PLACEMENT_3D('',#14306,#11385,#11386);
#9929=AXIS2_PLACEMENT_3D('',#14312,#11390,#11391);
#9930=AXIS2_PLACEMENT_3D('',#14313,#11392,#11393);
#9931=AXIS2_PLACEMENT_3D('',#14314,#11394,#11395);
#9932=AXIS2_PLACEMENT_3D('',#14315,#11396,#11397);
#9933=AXIS2_PLACEMENT_3D('',#14319,#11399,#11400);
#9934=AXIS2_PLACEMENT_3D('',#14320,#11401,#11402);
#9935=AXIS2_PLACEMENT_3D('',#14321,#11403,#11404);
#9936=AXIS2_PLACEMENT_3D('',#14324,#11407,#11408);
#9937=AXIS2_PLACEMENT_3D('',#14328,#11410,#11411);
#9938=AXIS2_PLACEMENT_3D('',#14329,#11412,#11413);
#9939=AXIS2_PLACEMENT_3D('',#14330,#11414,#11415);
#9940=AXIS2_PLACEMENT_3D('',#14336,#11419,#11420);
#9941=AXIS2_PLACEMENT_3D('',#14338,#11421,#11422);
#9942=AXIS2_PLACEMENT_3D('',#14341,#11424,#11425);
#9943=AXIS2_PLACEMENT_3D('',#14342,#11426,#11427);
#9944=AXIS2_PLACEMENT_3D('',#14346,#11429,#11430);
#9945=AXIS2_PLACEMENT_3D('',#14347,#11431,#11432);
#9946=AXIS2_PLACEMENT_3D('',#14348,#11433,#11434);
#9947=AXIS2_PLACEMENT_3D('',#14354,#11438,#11439);
#9948=AXIS2_PLACEMENT_3D('',#14359,#11441,#11442);
#9949=AXIS2_PLACEMENT_3D('',#14362,#11444,#11445);
#9950=AXIS2_PLACEMENT_3D('',#14363,#11446,#11447);
#9951=AXIS2_PLACEMENT_3D('',#14366,#11450,#11451);
#9952=AXIS2_PLACEMENT_3D('',#14370,#11453,#11454);
#9953=AXIS2_PLACEMENT_3D('',#14371,#11455,#11456);
#9954=AXIS2_PLACEMENT_3D('',#14372,#11457,#11458);
#9955=AXIS2_PLACEMENT_3D('',#14378,#11462,#11463);
#9956=AXIS2_PLACEMENT_3D('',#14383,#11465,#11466);
#9957=AXIS2_PLACEMENT_3D('',#14386,#11468,#11469);
#9958=AXIS2_PLACEMENT_3D('',#14387,#11470,#11471);
#9959=AXIS2_PLACEMENT_3D('',#14390,#11474,#11475);
#9960=AXIS2_PLACEMENT_3D('',#14395,#11479,#11480);
#9961=AXIS2_PLACEMENT_3D('',#14399,#11483,#11484);
#9962=AXIS2_PLACEMENT_3D('',#14402,#11487,#11488);
#9963=AXIS2_PLACEMENT_3D('',#14404,#11490,#11491);
#9964=AXIS2_PLACEMENT_3D('',#14406,#11493,#11494);
#9965=AXIS2_PLACEMENT_3D('',#14408,#11496,#11497);
#9966=AXIS2_PLACEMENT_3D('',#14410,#11499,#11500);
#9967=AXIS2_PLACEMENT_3D('',#14411,#11501,#11502);
#9968=AXIS2_PLACEMENT_3D('',#14413,#11504,#11505);
#9969=AXIS2_PLACEMENT_3D('',#14415,#11507,#11508);
#9970=AXIS2_PLACEMENT_3D('',#14417,#11510,#11511);
#9971=AXIS2_PLACEMENT_3D('',#14421,#11514,#11515);
#9972=AXIS2_PLACEMENT_3D('',#14425,#11518,#11519);
#9973=AXIS2_PLACEMENT_3D('',#14428,#11522,#11523);
#9974=AXIS2_PLACEMENT_3D('',#14430,#11525,#11526);
#9975=AXIS2_PLACEMENT_3D('',#14432,#11528,#11529);
#9976=AXIS2_PLACEMENT_3D('',#14435,#11532,#11533);
#9977=AXIS2_PLACEMENT_3D('',#14439,#11537,#11538);
#9978=AXIS2_PLACEMENT_3D('',#14441,#11540,#11541);
#9979=AXIS2_PLACEMENT_3D('',#14443,#11543,#11544);
#9980=AXIS2_PLACEMENT_3D('',#14445,#11546,#11547);
#9981=AXIS2_PLACEMENT_3D('',#14446,#11548,#11549);
#9982=AXIS2_PLACEMENT_3D('',#14447,#11550,#11551);
#9983=AXIS2_PLACEMENT_3D('',#14448,#11552,#11553);
#9984=AXIS2_PLACEMENT_3D('',#14450,#11554,#11555);
#9985=AXIS2_PLACEMENT_3D('',#14453,#11557,#11558);
#9986=AXIS2_PLACEMENT_3D('',#14454,#11559,#11560);
#9987=AXIS2_PLACEMENT_3D('',#14456,#11561,#11562);
#9988=AXIS2_PLACEMENT_3D('',#14458,#11563,#11564);
#9989=AXIS2_PLACEMENT_3D('',#14460,#11566,#11567);
#9990=AXIS2_PLACEMENT_3D('',#14462,#11569,#11570);
#9991=AXIS2_PLACEMENT_3D('',#14464,#11572,#11573);
#9992=AXIS2_PLACEMENT_3D('',#14470,#11577,#11578);
#9993=AXIS2_PLACEMENT_3D('',#14476,#11582,#11583);
#9994=AXIS2_PLACEMENT_3D('',#14482,#11587,#11588);
#9995=AXIS2_PLACEMENT_3D('',#14488,#11592,#11593);
#9996=AXIS2_PLACEMENT_3D('',#14490,#11595,#11596);
#9997=AXIS2_PLACEMENT_3D('',#14492,#11598,#11599);
#9998=AXIS2_PLACEMENT_3D('',#14493,#11600,#11601);
#9999=AXIS2_PLACEMENT_3D('',#14495,#11602,#11603);
#10000=AXIS2_PLACEMENT_3D('',#14497,#11604,#11605);
#10001=AXIS2_PLACEMENT_3D('',#14499,#11607,#11608);
#10002=AXIS2_PLACEMENT_3D('',#14501,#11609,#11610);
#10003=AXIS2_PLACEMENT_3D('',#14503,#11611,#11612);
#10004=AXIS2_PLACEMENT_3D('',#14505,#11614,#11615);
#10005=AXIS2_PLACEMENT_3D('',#14507,#11617,#11618);
#10006=AXIS2_PLACEMENT_3D('',#14509,#11620,#11621);
#10007=AXIS2_PLACEMENT_3D('',#14515,#11625,#11626);
#10008=AXIS2_PLACEMENT_3D('',#14521,#11630,#11631);
#10009=AXIS2_PLACEMENT_3D('',#14527,#11635,#11636);
#10010=AXIS2_PLACEMENT_3D('',#14533,#11640,#11641);
#10011=AXIS2_PLACEMENT_3D('',#14535,#11643,#11644);
#10012=AXIS2_PLACEMENT_3D('',#14537,#11646,#11647);
#10013=AXIS2_PLACEMENT_3D('',#14538,#11648,#11649);
#10014=AXIS2_PLACEMENT_3D('',#14539,#11650,#11651);
#10015=AXIS2_PLACEMENT_3D('',#14541,#11652,#11653);
#10016=AXIS2_PLACEMENT_3D('',#14544,#11655,#11656);
#10017=AXIS2_PLACEMENT_3D('',#14545,#11657,#11658);
#10018=AXIS2_PLACEMENT_3D('',#14547,#11659,#11660);
#10019=AXIS2_PLACEMENT_3D('',#14550,#11662,#11663);
#10020=AXIS2_PLACEMENT_3D('',#14551,#11664,#11665);
#10021=AXIS2_PLACEMENT_3D('',#14553,#11666,#11667);
#10022=AXIS2_PLACEMENT_3D('',#14556,#11669,#11670);
#10023=AXIS2_PLACEMENT_3D('',#14557,#11671,#11672);
#10024=AXIS2_PLACEMENT_3D('',#14559,#11673,#11674);
#10025=AXIS2_PLACEMENT_3D('',#14562,#11676,#11677);
#10026=AXIS2_PLACEMENT_3D('',#14563,#11678,#11679);
#10027=AXIS2_PLACEMENT_3D('',#14565,#11680,#11681);
#10028=AXIS2_PLACEMENT_3D('',#14568,#11683,#11684);
#10029=AXIS2_PLACEMENT_3D('',#14569,#11685,#11686);
#10030=AXIS2_PLACEMENT_3D('',#14571,#11687,#11688);
#10031=AXIS2_PLACEMENT_3D('',#14574,#11690,#11691);
#10032=AXIS2_PLACEMENT_3D('',#14575,#11692,#11693);
#10033=AXIS2_PLACEMENT_3D('',#14577,#11694,#11695);
#10034=AXIS2_PLACEMENT_3D('',#14580,#11697,#11698);
#10035=AXIS2_PLACEMENT_3D('',#14581,#11699,#11700);
#10036=AXIS2_PLACEMENT_3D('',#14583,#11701,#11702);
#10037=AXIS2_PLACEMENT_3D('',#14586,#11704,#11705);
#10038=AXIS2_PLACEMENT_3D('',#14587,#11706,#11707);
#10039=AXIS2_PLACEMENT_3D('',#14596,#11712,#11713);
#10040=AXIS2_PLACEMENT_3D('',#14601,#11715,#11716);
#10041=AXIS2_PLACEMENT_3D('',#14604,#11718,#11719);
#10042=AXIS2_PLACEMENT_3D('',#14605,#11720,#11721);
#10043=AXIS2_PLACEMENT_3D('',#14611,#11725,#11726);
#10044=AXIS2_PLACEMENT_3D('',#14616,#11728,#11729);
#10045=AXIS2_PLACEMENT_3D('',#14619,#11731,#11732);
#10046=AXIS2_PLACEMENT_3D('',#14620,#11733,#11734);
#10047=AXIS2_PLACEMENT_3D('',#14626,#11738,#11739);
#10048=AXIS2_PLACEMENT_3D('',#14631,#11741,#11742);
#10049=AXIS2_PLACEMENT_3D('',#14634,#11744,#11745);
#10050=AXIS2_PLACEMENT_3D('',#14635,#11746,#11747);
#10051=AXIS2_PLACEMENT_3D('',#14638,#11750,#11751);
#10052=AXIS2_PLACEMENT_3D('',#14639,#11752,#11753);
#10053=AXIS2_PLACEMENT_3D('',#14640,#11754,#11755);
#10054=AXIS2_PLACEMENT_3D('',#14641,#11756,#11757);
#10055=AXIS2_PLACEMENT_3D('',#14647,#11761,#11762);
#10056=AXIS2_PLACEMENT_3D('',#14656,#11767,#11768);
#10057=AXIS2_PLACEMENT_3D('',#14662,#11772,#11773);
#10058=AXIS2_PLACEMENT_3D('',#14668,#11777,#11778);
#10059=AXIS2_PLACEMENT_3D('',#14670,#11779,#11780);
#10060=AXIS2_PLACEMENT_3D('',#14673,#11782,#11783);
#10061=AXIS2_PLACEMENT_3D('',#14674,#11784,#11785);
#10062=AXIS2_PLACEMENT_3D('',#14682,#11791,#11792);
#10063=AXIS2_PLACEMENT_3D('',#14684,#11794,#11795);
#10064=AXIS2_PLACEMENT_3D('',#14686,#11797,#11798);
#10065=AXIS2_PLACEMENT_3D('',#14688,#11800,#11801);
#10066=AXIS2_PLACEMENT_3D('',#14692,#11804,#11805);
#10067=AXIS2_PLACEMENT_3D('',#14696,#11808,#11809);
#10068=AXIS2_PLACEMENT_3D('',#14699,#11812,#11813);
#10069=AXIS2_PLACEMENT_3D('',#14701,#11815,#11816);
#10070=AXIS2_PLACEMENT_3D('',#14703,#11818,#11819);
#10071=AXIS2_PLACEMENT_3D('',#14705,#11821,#11822);
#10072=AXIS2_PLACEMENT_3D('',#14715,#11828,#11829);
#10073=AXIS2_PLACEMENT_3D('',#14716,#11830,#11831);
#10074=AXIS2_PLACEMENT_3D('',#14717,#11832,#11833);
#10075=AXIS2_PLACEMENT_3D('',#14718,#11834,#11835);
#10076=AXIS2_PLACEMENT_3D('',#14719,#11836,#11837);
#10077=AXIS2_PLACEMENT_3D('',#14721,#11839,#11840);
#10078=AXIS2_PLACEMENT_3D('',#14722,#11841,#11842);
#10079=AXIS2_PLACEMENT_3D('',#14724,#11844,#11845);
#10080=AXIS2_PLACEMENT_3D('',#14725,#11846,#11847);
#10081=AXIS2_PLACEMENT_3D('',#14726,#11848,#11849);
#10082=AXIS2_PLACEMENT_3D('',#14728,#11850,#11851);
#10083=AXIS2_PLACEMENT_3D('',#14731,#11853,#11854);
#10084=AXIS2_PLACEMENT_3D('',#14732,#11855,#11856);
#10085=AXIS2_PLACEMENT_3D('',#14734,#11857,#11858);
#10086=AXIS2_PLACEMENT_3D('',#14737,#11860,#11861);
#10087=AXIS2_PLACEMENT_3D('',#14738,#11862,#11863);
#10088=AXIS2_PLACEMENT_3D('',#14740,#11864,#11865);
#10089=AXIS2_PLACEMENT_3D('',#14743,#11867,#11868);
#10090=AXIS2_PLACEMENT_3D('',#14744,#11869,#11870);
#10091=AXIS2_PLACEMENT_3D('',#14746,#11871,#11872);
#10092=AXIS2_PLACEMENT_3D('',#14749,#11874,#11875);
#10093=AXIS2_PLACEMENT_3D('',#14750,#11876,#11877);
#10094=AXIS2_PLACEMENT_3D('',#14752,#11878,#11879);
#10095=AXIS2_PLACEMENT_3D('',#14755,#11881,#11882);
#10096=AXIS2_PLACEMENT_3D('',#14756,#11883,#11884);
#10097=AXIS2_PLACEMENT_3D('',#14758,#11885,#11886);
#10098=AXIS2_PLACEMENT_3D('',#14761,#11888,#11889);
#10099=AXIS2_PLACEMENT_3D('',#14762,#11890,#11891);
#10100=AXIS2_PLACEMENT_3D('',#14764,#11892,#11893);
#10101=AXIS2_PLACEMENT_3D('',#14767,#11895,#11896);
#10102=AXIS2_PLACEMENT_3D('',#14768,#11897,#11898);
#10103=AXIS2_PLACEMENT_3D('',#14770,#11899,#11900);
#10104=AXIS2_PLACEMENT_3D('',#14773,#11902,#11903);
#10105=AXIS2_PLACEMENT_3D('',#14774,#11904,#11905);
#10106=AXIS2_PLACEMENT_3D('',#14783,#11910,#11911);
#10107=AXIS2_PLACEMENT_3D('',#14788,#11913,#11914);
#10108=AXIS2_PLACEMENT_3D('',#14791,#11916,#11917);
#10109=AXIS2_PLACEMENT_3D('',#14792,#11918,#11919);
#10110=AXIS2_PLACEMENT_3D('',#14798,#11923,#11924);
#10111=AXIS2_PLACEMENT_3D('',#14803,#11926,#11927);
#10112=AXIS2_PLACEMENT_3D('',#14806,#11929,#11930);
#10113=AXIS2_PLACEMENT_3D('',#14807,#11931,#11932);
#10114=AXIS2_PLACEMENT_3D('',#14813,#11936,#11937);
#10115=AXIS2_PLACEMENT_3D('',#14818,#11939,#11940);
#10116=AXIS2_PLACEMENT_3D('',#14821,#11942,#11943);
#10117=AXIS2_PLACEMENT_3D('',#14822,#11944,#11945);
#10118=AXIS2_PLACEMENT_3D('',#14825,#11948,#11949);
#10119=AXIS2_PLACEMENT_3D('',#14826,#11950,#11951);
#10120=AXIS2_PLACEMENT_3D('',#14827,#11952,#11953);
#10121=AXIS2_PLACEMENT_3D('',#14828,#11954,#11955);
#10122=AXIS2_PLACEMENT_3D('',#14834,#11959,#11960);
#10123=AXIS2_PLACEMENT_3D('',#14843,#11965,#11966);
#10124=AXIS2_PLACEMENT_3D('',#14849,#11970,#11971);
#10125=AXIS2_PLACEMENT_3D('',#14855,#11975,#11976);
#10126=AXIS2_PLACEMENT_3D('',#14857,#11977,#11978);
#10127=AXIS2_PLACEMENT_3D('',#14859,#11979,#11980);
#10128=AXIS2_PLACEMENT_3D('',#14861,#11982,#11983);
#10129=AXIS2_PLACEMENT_3D('',#14869,#11989,#11990);
#10130=AXIS2_PLACEMENT_3D('',#14871,#11992,#11993);
#10131=AXIS2_PLACEMENT_3D('',#14873,#11995,#11996);
#10132=AXIS2_PLACEMENT_3D('',#14875,#11998,#11999);
#10133=AXIS2_PLACEMENT_3D('',#14879,#12002,#12003);
#10134=AXIS2_PLACEMENT_3D('',#14883,#12006,#12007);
#10135=AXIS2_PLACEMENT_3D('',#14886,#12010,#12011);
#10136=AXIS2_PLACEMENT_3D('',#14888,#12013,#12014);
#10137=AXIS2_PLACEMENT_3D('',#14890,#12016,#12017);
#10138=AXIS2_PLACEMENT_3D('',#14892,#12019,#12020);
#10139=AXIS2_PLACEMENT_3D('',#14902,#12026,#12027);
#10140=AXIS2_PLACEMENT_3D('',#14903,#12028,#12029);
#10141=AXIS2_PLACEMENT_3D('',#14904,#12030,#12031);
#10142=AXIS2_PLACEMENT_3D('',#14905,#12032,#12033);
#10143=AXIS2_PLACEMENT_3D('',#14906,#12034,#12035);
#10144=AXIS2_PLACEMENT_3D('',#14908,#12037,#12038);
#10145=AXIS2_PLACEMENT_3D('',#14909,#12039,#12040);
#10146=AXIS2_PLACEMENT_3D('',#14911,#12042,#12043);
#10147=AXIS2_PLACEMENT_3D('',#14912,#12044,#12045);
#10148=AXIS2_PLACEMENT_3D('',#14913,#12046,#12047);
#10149=AXIS2_PLACEMENT_3D('',#14915,#12048,#12049);
#10150=AXIS2_PLACEMENT_3D('',#14918,#12051,#12052);
#10151=AXIS2_PLACEMENT_3D('',#14919,#12053,#12054);
#10152=AXIS2_PLACEMENT_3D('',#14921,#12055,#12056);
#10153=AXIS2_PLACEMENT_3D('',#14924,#12058,#12059);
#10154=AXIS2_PLACEMENT_3D('',#14925,#12060,#12061);
#10155=AXIS2_PLACEMENT_3D('',#14927,#12062,#12063);
#10156=AXIS2_PLACEMENT_3D('',#14930,#12065,#12066);
#10157=AXIS2_PLACEMENT_3D('',#14931,#12067,#12068);
#10158=AXIS2_PLACEMENT_3D('',#14936,#12070,#12071);
#10159=AXIS2_PLACEMENT_3D('',#14939,#12073,#12074);
#10160=AXIS2_PLACEMENT_3D('',#14940,#12075,#12076);
#10161=AXIS2_PLACEMENT_3D('',#14946,#12080,#12081);
#10162=AXIS2_PLACEMENT_3D('',#14951,#12083,#12084);
#10163=AXIS2_PLACEMENT_3D('',#14954,#12086,#12087);
#10164=AXIS2_PLACEMENT_3D('',#14955,#12088,#12089);
#10165=AXIS2_PLACEMENT_3D('',#14961,#12093,#12094);
#10166=AXIS2_PLACEMENT_3D('',#14965,#12096,#12097);
#10167=AXIS2_PLACEMENT_3D('',#14966,#12098,#12099);
#10168=AXIS2_PLACEMENT_3D('',#14967,#12100,#12101);
#10169=AXIS2_PLACEMENT_3D('',#14973,#12105,#12106);
#10170=AXIS2_PLACEMENT_3D('',#14978,#12108,#12109);
#10171=AXIS2_PLACEMENT_3D('',#14981,#12111,#12112);
#10172=AXIS2_PLACEMENT_3D('',#14982,#12113,#12114);
#10173=AXIS2_PLACEMENT_3D('',#14985,#12117,#12118);
#10174=AXIS2_PLACEMENT_3D('',#14989,#12120,#12121);
#10175=AXIS2_PLACEMENT_3D('',#14990,#12122,#12123);
#10176=AXIS2_PLACEMENT_3D('',#14991,#12124,#12125);
#10177=AXIS2_PLACEMENT_3D('',#14997,#12129,#12130);
#10178=AXIS2_PLACEMENT_3D('',#15002,#12132,#12133);
#10179=AXIS2_PLACEMENT_3D('',#15005,#12135,#12136);
#10180=AXIS2_PLACEMENT_3D('',#15006,#12137,#12138);
#10181=AXIS2_PLACEMENT_3D('',#15009,#12141,#12142);
#10182=AXIS2_PLACEMENT_3D('',#15015,#12146,#12147);
#10183=AXIS2_PLACEMENT_3D('',#15024,#12152,#12153);
#10184=AXIS2_PLACEMENT_3D('',#15030,#12157,#12158);
#10185=AXIS2_PLACEMENT_3D('',#15036,#12162,#12163);
#10186=AXIS2_PLACEMENT_3D('',#15038,#12164,#12165);
#10187=AXIS2_PLACEMENT_3D('',#15040,#12166,#12167);
#10188=AXIS2_PLACEMENT_3D('',#15042,#12169,#12170);
#10189=AXIS2_PLACEMENT_3D('',#15050,#12176,#12177);
#10190=AXIS2_PLACEMENT_3D('',#15052,#12179,#12180);
#10191=AXIS2_PLACEMENT_3D('',#15054,#12182,#12183);
#10192=AXIS2_PLACEMENT_3D('',#15056,#12185,#12186);
#10193=AXIS2_PLACEMENT_3D('',#15058,#12188,#12189);
#10194=AXIS2_PLACEMENT_3D('',#15060,#12191,#12192);
#10195=AXIS2_PLACEMENT_3D('',#15064,#12195,#12196);
#10196=AXIS2_PLACEMENT_3D('',#15068,#12199,#12200);
#10197=AXIS2_PLACEMENT_3D('',#15071,#12203,#12204);
#10198=AXIS2_PLACEMENT_3D('',#15073,#12206,#12207);
#10199=AXIS2_PLACEMENT_3D('',#15075,#12209,#12210);
#10200=AXIS2_PLACEMENT_3D('',#15077,#12212,#12213);
#10201=AXIS2_PLACEMENT_3D('',#15079,#12215,#12216);
#10202=AXIS2_PLACEMENT_3D('',#15081,#12218,#12219);
#10203=AXIS2_PLACEMENT_3D('',#15091,#12225,#12226);
#10204=AXIS2_PLACEMENT_3D('',#15092,#12227,#12228);
#10205=AXIS2_PLACEMENT_3D('',#15093,#12229,#12230);
#10206=AXIS2_PLACEMENT_3D('',#15094,#12231,#12232);
#10207=AXIS2_PLACEMENT_3D('',#15095,#12233,#12234);
#10208=AXIS2_PLACEMENT_3D('',#15097,#12236,#12237);
#10209=AXIS2_PLACEMENT_3D('',#15098,#12238,#12239);
#10210=AXIS2_PLACEMENT_3D('',#15100,#12241,#12242);
#10211=AXIS2_PLACEMENT_3D('',#15101,#12243,#12244);
#10212=AXIS2_PLACEMENT_3D('',#15102,#12245,#12246);
#10213=AXIS2_PLACEMENT_3D('',#15107,#12248,#12249);
#10214=AXIS2_PLACEMENT_3D('',#15110,#12251,#12252);
#10215=AXIS2_PLACEMENT_3D('',#15111,#12253,#12254);
#10216=AXIS2_PLACEMENT_3D('',#15117,#12258,#12259);
#10217=AXIS2_PLACEMENT_3D('',#15122,#12261,#12262);
#10218=AXIS2_PLACEMENT_3D('',#15125,#12264,#12265);
#10219=AXIS2_PLACEMENT_3D('',#15126,#12266,#12267);
#10220=AXIS2_PLACEMENT_3D('',#15132,#12271,#12272);
#10221=AXIS2_PLACEMENT_3D('',#15136,#12274,#12275);
#10222=AXIS2_PLACEMENT_3D('',#15137,#12276,#12277);
#10223=AXIS2_PLACEMENT_3D('',#15138,#12278,#12279);
#10224=AXIS2_PLACEMENT_3D('',#15144,#12283,#12284);
#10225=AXIS2_PLACEMENT_3D('',#15149,#12286,#12287);
#10226=AXIS2_PLACEMENT_3D('',#15152,#12289,#12290);
#10227=AXIS2_PLACEMENT_3D('',#15153,#12291,#12292);
#10228=AXIS2_PLACEMENT_3D('',#15156,#12295,#12296);
#10229=AXIS2_PLACEMENT_3D('',#15161,#12300,#12301);
#10230=AXIS2_PLACEMENT_3D('',#15165,#12304,#12305);
#10231=AXIS2_PLACEMENT_3D('',#15168,#12308,#12309);
#10232=AXIS2_PLACEMENT_3D('',#15170,#12311,#12312);
#10233=AXIS2_PLACEMENT_3D('',#15172,#12314,#12315);
#10234=AXIS2_PLACEMENT_3D('',#15174,#12317,#12318);
#10235=AXIS2_PLACEMENT_3D('',#15178,#12321,#12322);
#10236=AXIS2_PLACEMENT_3D('',#15182,#12325,#12326);
#10237=AXIS2_PLACEMENT_3D('',#15185,#12329,#12330);
#10238=AXIS2_PLACEMENT_3D('',#15187,#12332,#12333);
#10239=AXIS2_PLACEMENT_3D('',#15189,#12335,#12336);
#10240=AXIS2_PLACEMENT_3D('',#15190,#12337,#12338);
#10241=AXIS2_PLACEMENT_3D('',#15191,#12339,#12340);
#10242=AXIS2_PLACEMENT_3D('',#15192,#12341,#12342);
#10243=AXIS2_PLACEMENT_3D('',#15193,#12343,#12344);
#10244=AXIS2_PLACEMENT_3D('',#15194,#12345,#12346);
#10245=AXIS2_PLACEMENT_3D('',#15195,#12347,#12348);
#10246=AXIS2_PLACEMENT_3D('',#15198,#12349,#12350);
#10247=AXIS2_PLACEMENT_3D('',#15215,#12351,#12352);
#10248=AXIS2_PLACEMENT_3D('',#15230,#12353,#12354);
#10249=AXIS2_PLACEMENT_3D('',#15233,#12355,#12356);
#10250=AXIS2_PLACEMENT_3D('',#15252,#12359,#12360);
#10251=AXIS2_PLACEMENT_3D('',#15254,#12361,#12362);
#10252=AXIS2_PLACEMENT_3D('',#15256,#12363,#12364);
#10253=AXIS2_PLACEMENT_3D('',#15272,#12365,#12366);
#10254=AXIS2_PLACEMENT_3D('',#15285,#12367,#12368);
#10255=AXIS2_PLACEMENT_3D('',#15287,#12369,#12370);
#10256=AXIS2_PLACEMENT_3D('',#15289,#12371,#12372);
#10257=AXIS2_PLACEMENT_3D('',#15291,#12373,#12374);
#10258=AXIS2_PLACEMENT_3D('',#15293,#12375,#12376);
#10259=AXIS2_PLACEMENT_3D('',#15305,#12377,#12378);
#10260=AXIS2_PLACEMENT_3D('',#15322,#12379,#12380);
#10261=AXIS2_PLACEMENT_3D('',#15335,#12381,#12382);
#10262=AXIS2_PLACEMENT_3D('',#15350,#12383,#12384);
#10263=AXIS2_PLACEMENT_3D('',#15362,#12385,#12386);
#10264=AXIS2_PLACEMENT_3D('',#15365,#12387,#12388);
#10265=AXIS2_PLACEMENT_3D('',#15367,#12389,#12390);
#10266=AXIS2_PLACEMENT_3D('',#15369,#12391,#12392);
#10267=AXIS2_PLACEMENT_3D('',#15370,#12393,#12394);
#10268=AXIS2_PLACEMENT_3D('',#15387,#12395,#12396);
#10269=AXIS2_PLACEMENT_3D('',#15400,#12397,#12398);
#10270=AXIS2_PLACEMENT_3D('',#15415,#12399,#12400);
#10271=AXIS2_PLACEMENT_3D('',#15428,#12401,#12402);
#10272=AXIS2_PLACEMENT_3D('',#15430,#12403,#12404);
#10273=AXIS2_PLACEMENT_3D('',#15432,#12405,#12406);
#10274=AXIS2_PLACEMENT_3D('',#15445,#12407,#12408);
#10275=AXIS2_PLACEMENT_3D('',#15460,#12409,#12410);
#10276=AXIS2_PLACEMENT_3D('',#15473,#12411,#12412);
#10277=AXIS2_PLACEMENT_3D('',#15489,#12413,#12414);
#10278=AXIS2_PLACEMENT_3D('',#15491,#12415,#12416);
#10279=AXIS2_PLACEMENT_3D('',#15492,#12417,#12418);
#10280=AXIS2_PLACEMENT_3D('',#15509,#12419,#12420);
#10281=AXIS2_PLACEMENT_3D('',#15522,#12421,#12422);
#10282=AXIS2_PLACEMENT_3D('',#15537,#12423,#12424);
#10283=AXIS2_PLACEMENT_3D('',#15549,#12425,#12426);
#10284=AXIS2_PLACEMENT_3D('',#15565,#12427,#12428);
#10285=AXIS2_PLACEMENT_3D('',#15578,#12429,#12430);
#10286=AXIS2_PLACEMENT_3D('',#15594,#12431,#12432);
#10287=AXIS2_PLACEMENT_3D('',#15596,#12433,#12434);
#10288=AXIS2_PLACEMENT_3D('',#15598,#12435,#12436);
#10289=AXIS2_PLACEMENT_3D('',#15650,#12437,#12438);
#10290=AXIS2_PLACEMENT_3D('',#15684,#12439,#12440);
#10291=AXIS2_PLACEMENT_3D('',#15699,#12441,#12442);
#10292=AXIS2_PLACEMENT_3D('',#15715,#12443,#12444);
#10293=AXIS2_PLACEMENT_3D('',#15728,#12445,#12446);
#10294=AXIS2_PLACEMENT_3D('',#15743,#12447,#12448);
#10295=AXIS2_PLACEMENT_3D('',#15745,#12449,#12450);
#10296=AXIS2_PLACEMENT_3D('',#15747,#12451,#12452);
#10297=AXIS2_PLACEMENT_3D('',#15762,#12453,#12454);
#10298=AXIS2_PLACEMENT_3D('',#15796,#12455,#12456);
#10299=AXIS2_PLACEMENT_3D('',#15844,#12457,#12458);
#10300=AXIS2_PLACEMENT_3D('',#15845,#12459,#12460);
#10301=AXIS2_PLACEMENT_3D('',#15862,#12463,#12464);
#10302=AXIS2_PLACEMENT_3D('',#15893,#12467,#12468);
#10303=AXIS2_PLACEMENT_3D('',#15910,#12471,#12472);
#10304=AXIS2_PLACEMENT_3D('',#15927,#12475,#12476);
#10305=AXIS2_PLACEMENT_3D('',#15958,#12479,#12480);
#10306=AXIS2_PLACEMENT_3D('',#15975,#12483,#12484);
#10307=AXIS2_PLACEMENT_3D('',#15992,#12487,#12488);
#10308=AXIS2_PLACEMENT_3D('',#16009,#12491,#12492);
#10309=AXIS2_PLACEMENT_3D('',#16026,#12495,#12496);
#10310=AXIS2_PLACEMENT_3D('',#16043,#12499,#12500);
#10311=AXIS2_PLACEMENT_3D('',#16045,#12501,#12502);
#10312=AXIS2_PLACEMENT_3D('',#16048,#12504,#12505);
#10313=AXIS2_PLACEMENT_3D('',#16049,#12506,#12507);
#10314=AXIS2_PLACEMENT_3D('',#16052,#12508,#12509);
#10315=AXIS2_PLACEMENT_3D('',#16069,#12510,#12511);
#10316=AXIS2_PLACEMENT_3D('',#16084,#12512,#12513);
#10317=AXIS2_PLACEMENT_3D('',#16088,#12515,#12516);
#10318=AXIS2_PLACEMENT_3D('',#16090,#12518,#12519);
#10319=AXIS2_PLACEMENT_3D('',#16092,#12520,#12521);
#10320=AXIS2_PLACEMENT_3D('',#16095,#12523,#12524);
#10321=AXIS2_PLACEMENT_3D('',#16096,#12525,#12526);
#10322=AXIS2_PLACEMENT_3D('',#16098,#12527,#12528);
#10323=AXIS2_PLACEMENT_3D('',#16101,#12530,#12531);
#10324=AXIS2_PLACEMENT_3D('',#16102,#12532,#12533);
#10325=AXIS2_PLACEMENT_3D('',#16113,#12540,#12541);
#10326=AXIS2_PLACEMENT_3D('',#16120,#12544,#12545);
#10327=AXIS2_PLACEMENT_3D('',#16124,#12547,#12548);
#10328=AXIS2_PLACEMENT_3D('',#16132,#12552,#12553);
#10329=AXIS2_PLACEMENT_3D('',#16136,#12555,#12556);
#10330=AXIS2_PLACEMENT_3D('',#16138,#12558,#12559);
#10331=AXIS2_PLACEMENT_3D('',#16139,#12560,#12561);
#10332=AXIS2_PLACEMENT_3D('',#16140,#12562,#12563);
#10333=AXIS2_PLACEMENT_3D('',#16141,#12564,#12565);
#10334=AXIS2_PLACEMENT_3D('',#16142,#12566,#12567);
#10335=AXIS2_PLACEMENT_3D('',#16143,#12568,#12569);
#10336=AXIS2_PLACEMENT_3D('',#16144,#12570,#12571);
#10337=AXIS2_PLACEMENT_3D('',#16147,#12574,#12575);
#10338=AXIS2_PLACEMENT_3D('',#16149,#12577,#12578);
#10339=AXIS2_PLACEMENT_3D('',#16151,#12580,#12581);
#10340=AXIS2_PLACEMENT_3D('',#16154,#12584,#12585);
#10341=AXIS2_PLACEMENT_3D('',#16157,#12588,#12589);
#10342=AXIS2_PLACEMENT_3D('',#16158,#12590,#12591);
#10343=AXIS2_PLACEMENT_3D('',#16159,#12592,#12593);
#10344=AXIS2_PLACEMENT_3D('',#16160,#12594,#12595);
#10345=AXIS2_PLACEMENT_3D('',#16196,#12598,#12599);
#10346=AXIS2_PLACEMENT_3D('',#16197,#12600,#12601);
#10347=AXIS2_PLACEMENT_3D('',#16198,#12602,#12603);
#10348=AXIS2_PLACEMENT_3D('',#16249,#12606,#12607);
#10349=AXIS2_PLACEMENT_3D('',#16250,#12608,#12609);
#10350=AXIS2_PLACEMENT_3D('',#16251,#12610,#12611);
#10351=AXIS2_PLACEMENT_3D('',#16266,#12614,#12615);
#10352=AXIS2_PLACEMENT_3D('',#16284,#12618,#12619);
#10353=AXIS2_PLACEMENT_3D('',#16338,#12622,#12623);
#10354=AXIS2_PLACEMENT_3D('',#16341,#12625,#12626);
#10355=AXIS2_PLACEMENT_3D('',#16342,#12627,#12628);
#10356=AXIS2_PLACEMENT_3D('',#16345,#12630,#12631);
#10357=AXIS2_PLACEMENT_3D('',#16346,#12632,#12633);
#10358=AXIS2_PLACEMENT_3D('',#16347,#12634,#12635);
#10359=AXIS2_PLACEMENT_3D('',#16348,#12636,#12637);
#10360=AXIS2_PLACEMENT_3D('',#16384,#12640,#12641);
#10361=AXIS2_PLACEMENT_3D('',#16385,#12642,#12643);
#10362=AXIS2_PLACEMENT_3D('',#16386,#12644,#12645);
#10363=AXIS2_PLACEMENT_3D('',#16387,#12646,#12647);
#10364=AXIS2_PLACEMENT_3D('',#16388,#12648,#12649);
#10365=AXIS2_PLACEMENT_3D('',#16406,#12652,#12653);
#10366=AXIS2_PLACEMENT_3D('',#16421,#12656,#12657);
#10367=AXIS2_PLACEMENT_3D('',#16424,#12659,#12660);
#10368=AXIS2_PLACEMENT_3D('',#16425,#12661,#12662);
#10369=AXIS2_PLACEMENT_3D('',#16428,#12664,#12665);
#10370=AXIS2_PLACEMENT_3D('',#16429,#12666,#12667);
#10371=AXIS2_PLACEMENT_3D('',#16430,#12668,#12669);
#10372=AXIS2_PLACEMENT_3D('',#16431,#12670,#12671);
#10373=AXIS2_PLACEMENT_3D('',#16432,#12672,#12673);
#10374=AXIS2_PLACEMENT_3D('',#16433,#12674,#12675);
#10375=AXIS2_PLACEMENT_3D('',#16434,#12676,#12677);
#10376=AXIS2_PLACEMENT_3D('',#16435,#12678,#12679);
#10377=AXIS2_PLACEMENT_3D('',#16436,#12680,#12681);
#10378=AXIS2_PLACEMENT_3D('',#16437,#12682,#12683);
#10379=AXIS2_PLACEMENT_3D('',#16438,#12684,#12685);
#10380=AXIS2_PLACEMENT_3D('',#16439,#12686,#12687);
#10381=AXIS2_PLACEMENT_3D('',#16440,#12688,#12689);
#10382=AXIS2_PLACEMENT_3D('',#16441,#12690,#12691);
#10383=AXIS2_PLACEMENT_3D('',#16442,#12692,#12693);
#10384=AXIS2_PLACEMENT_3D('',#16443,#12694,#12695);
#10385=AXIS2_PLACEMENT_3D('',#16444,#12696,#12697);
#10386=AXIS2_PLACEMENT_3D('',#16459,#12700,#12701);
#10387=AXIS2_PLACEMENT_3D('',#16477,#12704,#12705);
#10388=AXIS2_PLACEMENT_3D('',#16492,#12708,#12709);
#10389=AXIS2_PLACEMENT_3D('',#16493,#12710,#12711);
#10390=AXIS2_PLACEMENT_3D('',#16494,#12712,#12713);
#10391=AXIS2_PLACEMENT_3D('',#16495,#12714,#12715);
#10392=AXIS2_PLACEMENT_3D('',#16496,#12716,#12717);
#10393=AXIS2_PLACEMENT_3D('',#16497,#12718,#12719);
#10394=AXIS2_PLACEMENT_3D('',#16498,#12720,#12721);
#10395=AXIS2_PLACEMENT_3D('',#16499,#12722,#12723);
#10396=AXIS2_PLACEMENT_3D('',#16500,#12724,#12725);
#10397=AXIS2_PLACEMENT_3D('',#16502,#12726,#12727);
#10398=AXIS2_PLACEMENT_3D('',#16504,#12728,#12729);
#10399=AXIS2_PLACEMENT_3D('',#16538,#12730,#12731);
#10400=AXIS2_PLACEMENT_3D('',#16590,#12732,#12733);
#10401=AXIS2_PLACEMENT_3D('',#16622,#12734,#12735);
#10402=AXIS2_PLACEMENT_3D('',#16625,#12737,#12738);
#10403=AXIS2_PLACEMENT_3D('',#16626,#12739,#12740);
#10404=AXIS2_PLACEMENT_3D('',#16628,#12741,#12742);
#10405=AXIS2_PLACEMENT_3D('',#16630,#12744,#12745);
#10406=AXIS2_PLACEMENT_3D('',#16664,#12747,#12748);
#10407=AXIS2_PLACEMENT_3D('',#16666,#12749,#12750);
#10408=AXIS2_PLACEMENT_3D('',#16668,#12752,#12753);
#10409=AXIS2_PLACEMENT_3D('',#16720,#12755,#12756);
#10410=AXIS2_PLACEMENT_3D('',#16722,#12757,#12758);
#10411=AXIS2_PLACEMENT_3D('',#16724,#12760,#12761);
#10412=AXIS2_PLACEMENT_3D('',#16759,#12762,#12763);
#10413=AXIS2_PLACEMENT_3D('',#16760,#12764,#12765);
#10414=AXIS2_PLACEMENT_3D('',#16775,#12768,#12769);
#10415=AXIS2_PLACEMENT_3D('',#16793,#12772,#12773);
#10416=AXIS2_PLACEMENT_3D('',#16811,#12776,#12777);
#10417=AXIS2_PLACEMENT_3D('',#16814,#12779,#12780);
#10418=AXIS2_PLACEMENT_3D('',#16815,#12781,#12782);
#10419=AXIS2_PLACEMENT_3D('',#16818,#12784,#12785);
#10420=AXIS2_PLACEMENT_3D('',#16819,#12786,#12787);
#10421=AXIS2_PLACEMENT_3D('',#16820,#12788,#12789);
#10422=AXIS2_PLACEMENT_3D('',#16821,#12790,#12791);
#10423=AXIS2_PLACEMENT_3D('',#16836,#12794,#12795);
#10424=AXIS2_PLACEMENT_3D('',#16837,#12796,#12797);
#10425=AXIS2_PLACEMENT_3D('',#16838,#12798,#12799);
#10426=AXIS2_PLACEMENT_3D('',#16839,#12800,#12801);
#10427=AXIS2_PLACEMENT_3D('',#16840,#12802,#12803);
#10428=AXIS2_PLACEMENT_3D('',#16855,#12806,#12807);
#10429=AXIS2_PLACEMENT_3D('',#16856,#12808,#12809);
#10430=AXIS2_PLACEMENT_3D('',#16857,#12810,#12811);
#10431=AXIS2_PLACEMENT_3D('',#16872,#12814,#12815);
#10432=AXIS2_PLACEMENT_3D('',#16873,#12816,#12817);
#10433=AXIS2_PLACEMENT_3D('',#16874,#12818,#12819);
#10434=AXIS2_PLACEMENT_3D('',#16875,#12820,#12821);
#10435=AXIS2_PLACEMENT_3D('',#16876,#12822,#12823);
#10436=AXIS2_PLACEMENT_3D('',#16879,#12825,#12826);
#10437=AXIS2_PLACEMENT_3D('',#16880,#12827,#12828);
#10438=AXIS2_PLACEMENT_3D('',#16883,#12830,#12831);
#10439=AXIS2_PLACEMENT_3D('',#16884,#12832,#12833);
#10440=AXIS2_PLACEMENT_3D('',#16885,#12834,#12835);
#10441=AXIS2_PLACEMENT_3D('',#16886,#12836,#12837);
#10442=AXIS2_PLACEMENT_3D('',#16887,#12838,#12839);
#10443=AXIS2_PLACEMENT_3D('',#16888,#12840,#12841);
#10444=AXIS2_PLACEMENT_3D('',#16889,#12842,#12843);
#10445=AXIS2_PLACEMENT_3D('',#16904,#12846,#12847);
#10446=AXIS2_PLACEMENT_3D('',#16922,#12850,#12851);
#10447=AXIS2_PLACEMENT_3D('',#16940,#12854,#12855);
#10448=AXIS2_PLACEMENT_3D('',#16943,#12857,#12858);
#10449=AXIS2_PLACEMENT_3D('',#16944,#12859,#12860);
#10450=AXIS2_PLACEMENT_3D('',#16947,#12862,#12863);
#10451=AXIS2_PLACEMENT_3D('',#16948,#12864,#12865);
#10452=AXIS2_PLACEMENT_3D('',#16949,#12866,#12867);
#10453=AXIS2_PLACEMENT_3D('',#16950,#12868,#12869);
#10454=AXIS2_PLACEMENT_3D('',#16965,#12872,#12873);
#10455=AXIS2_PLACEMENT_3D('',#16966,#12874,#12875);
#10456=AXIS2_PLACEMENT_3D('',#16967,#12876,#12877);
#10457=AXIS2_PLACEMENT_3D('',#16972,#12880,#12881);
#10458=AXIS2_PLACEMENT_3D('',#16973,#12882,#12883);
#10459=AXIS2_PLACEMENT_3D('',#16976,#12885,#12886);
#10460=AXIS2_PLACEMENT_3D('',#16977,#12887,#12888);
#10461=AXIS2_PLACEMENT_3D('',#16978,#12889,#12890);
#10462=AXIS2_PLACEMENT_3D('',#16979,#12891,#12892);
#10463=AXIS2_PLACEMENT_3D('',#16982,#12894,#12895);
#10464=AXIS2_PLACEMENT_3D('',#16983,#12896,#12897);
#10465=AXIS2_PLACEMENT_3D('',#16984,#12898,#12899);
#10466=AXIS2_PLACEMENT_3D('',#16985,#12900,#12901);
#10467=AXIS2_PLACEMENT_3D('',#16986,#12902,#12903);
#10468=AXIS2_PLACEMENT_3D('',#16987,#12904,#12905);
#10469=AXIS2_PLACEMENT_3D('',#16988,#12906,#12907);
#10470=AXIS2_PLACEMENT_3D('',#16993,#12910,#12911);
#10471=AXIS2_PLACEMENT_3D('',#16994,#12912,#12913);
#10472=AXIS2_PLACEMENT_3D('',#16997,#12915,#12916);
#10473=AXIS2_PLACEMENT_3D('',#16998,#12917,#12918);
#10474=AXIS2_PLACEMENT_3D('',#17001,#12920,#12921);
#10475=AXIS2_PLACEMENT_3D('',#17002,#12922,#12923);
#10476=AXIS2_PLACEMENT_3D('',#17003,#12924,#12925);
#10477=AXIS2_PLACEMENT_3D('',#17004,#12926,#12927);
#10478=AXIS2_PLACEMENT_3D('',#17005,#12928,#12929);
#10479=AXIS2_PLACEMENT_3D('',#17007,#12930,#12931);
#10480=AXIS2_PLACEMENT_3D('',#17009,#12932,#12933);
#10481=AXIS2_PLACEMENT_3D('',#17011,#12935,#12936);
#10482=AXIS2_PLACEMENT_3D('',#17080,#12938,#12939);
#10483=AXIS2_PLACEMENT_3D('',#17082,#12940,#12941);
#10484=AXIS2_PLACEMENT_3D('',#17084,#12942,#12943);
#10485=AXIS2_PLACEMENT_3D('',#17086,#12945,#12946);
#10486=AXIS2_PLACEMENT_3D('',#17116,#12948,#12949);
#10487=AXIS2_PLACEMENT_3D('',#17118,#12950,#12951);
#10488=AXIS2_PLACEMENT_3D('',#17120,#12952,#12953);
#10489=AXIS2_PLACEMENT_3D('',#17122,#12955,#12956);
#10490=AXIS2_PLACEMENT_3D('',#17191,#12958,#12959);
#10491=AXIS2_PLACEMENT_3D('',#17192,#12960,#12961);
#10492=AXIS2_PLACEMENT_3D('',#17193,#12962,#12963);
#10493=AXIS2_PLACEMENT_3D('',#17194,#12964,#12965);
#10494=AXIS2_PLACEMENT_3D('',#17195,#12966,#12967);
#10495=AXIS2_PLACEMENT_3D('',#17197,#12968,#12969);
#10496=AXIS2_PLACEMENT_3D('',#17199,#12970,#12971);
#10497=AXIS2_PLACEMENT_3D('',#17212,#12972,#12973);
#10498=AXIS2_PLACEMENT_3D('',#17228,#12974,#12975);
#10499=AXIS2_PLACEMENT_3D('',#17239,#12976,#12977);
#10500=AXIS2_PLACEMENT_3D('',#17241,#12979,#12980);
#10501=AXIS2_PLACEMENT_3D('',#17244,#12983,#12984);
#10502=AXIS2_PLACEMENT_3D('',#17247,#12987,#12988);
#10503=AXIS2_PLACEMENT_3D('',#17249,#12990,#12991);
#10504=AXIS2_PLACEMENT_3D('',#17250,#12992,#12993);
#10505=AXIS2_PLACEMENT_3D('',#17251,#12994,#12995);
#10506=AXIS2_PLACEMENT_3D('',#17252,#12996,#12997);
#10507=AXIS2_PLACEMENT_3D('',#17253,#12998,#12999);
#10508=AXIS2_PLACEMENT_3D('',#17254,#13000,#13001);
#10509=AXIS2_PLACEMENT_3D('',#17255,#13002,#13003);
#10510=AXIS2_PLACEMENT_3D('',#17257,#13004,#13005);
#10511=AXIS2_PLACEMENT_3D('',#17259,#13006,#13007);
#10512=AXIS2_PLACEMENT_3D('',#17260,#13008,#13009);
#10513=AXIS2_PLACEMENT_3D('',#17261,#13010,#13011);
#10514=AXIS2_PLACEMENT_3D('',#17263,#13012,#13013);
#10515=AXIS2_PLACEMENT_3D('',#17265,#13015,#13016);
#10516=AXIS2_PLACEMENT_3D('',#17267,#13017,#13018);
#10517=AXIS2_PLACEMENT_3D('',#17268,#13019,#13020);
#10518=AXIS2_PLACEMENT_3D('',#17269,#13021,#13022);
#10519=AXIS2_PLACEMENT_3D('',#17272,#13023,#13024);
#10520=AXIS2_PLACEMENT_3D('',#17273,#13025,#13026);
#10521=AXIS2_PLACEMENT_3D('',#17276,#13028,#13029);
#10522=AXIS2_PLACEMENT_3D('',#17277,#13030,#13031);
#10523=AXIS2_PLACEMENT_3D('',#17280,#13033,#13034);
#10524=AXIS2_PLACEMENT_3D('',#17281,#13035,#13036);
#10525=AXIS2_PLACEMENT_3D('',#17291,#13037,#13038);
#10526=AXIS2_PLACEMENT_3D('',#17292,#13039,#13040);
#10527=AXIS2_PLACEMENT_3D('',#17295,#13041,#13042);
#10528=AXIS2_PLACEMENT_3D('',#17297,#13043,#13044);
#10529=AXIS2_PLACEMENT_3D('',#17298,#13045,#13046);
#10530=AXIS2_PLACEMENT_3D('',#17300,#13047,#13048);
#10531=AXIS2_PLACEMENT_3D('',#17301,#13049,#13050);
#10532=AXIS2_PLACEMENT_3D('',#17302,#13051,#13052);
#10533=AXIS2_PLACEMENT_3D('',#17310,#13053,#13054);
#10534=AXIS2_PLACEMENT_3D('',#17318,#13055,#13056);
#10535=AXIS2_PLACEMENT_3D('',#17326,#13057,#13058);
#10536=AXIS2_PLACEMENT_3D('',#17334,#13059,#13060);
#10537=AXIS2_PLACEMENT_3D('',#17342,#13061,#13062);
#10538=AXIS2_PLACEMENT_3D('',#17348,#13066,#13067);
#10539=AXIS2_PLACEMENT_3D('',#17352,#13070,#13071);
#10540=AXIS2_PLACEMENT_3D('',#17356,#13074,#13075);
#10541=AXIS2_PLACEMENT_3D('',#17360,#13078,#13079);
#10542=AXIS2_PLACEMENT_3D('',#17364,#13082,#13083);
#10543=AXIS2_PLACEMENT_3D('',#17366,#13085,#13086);
#10544=AXIS2_PLACEMENT_3D('',#17367,#13087,#13088);
#10545=AXIS2_PLACEMENT_3D('',#17368,#13089,#13090);
#10546=AXIS2_PLACEMENT_3D('',#17369,#13091,#13092);
#10547=AXIS2_PLACEMENT_3D('',#17370,#13093,#13094);
#10548=AXIS2_PLACEMENT_3D('',#17372,#13095,#13096);
#10549=AXIS2_PLACEMENT_3D('',#17375,#13098,#13099);
#10550=AXIS2_PLACEMENT_3D('',#17376,#13100,#13101);
#10551=AXIS2_PLACEMENT_3D('',#17378,#13102,#13103);
#10552=AXIS2_PLACEMENT_3D('',#17380,#13104,#13105);
#10553=AXIS2_PLACEMENT_3D('',#17382,#13106,#13107);
#10554=AXIS2_PLACEMENT_3D('',#17383,#13108,#13109);
#10555=AXIS2_PLACEMENT_3D('',#17384,#13110,#13111);
#10556=AXIS2_PLACEMENT_3D('',#17387,#13112,#13113);
#10557=AXIS2_PLACEMENT_3D('',#17388,#13114,#13115);
#10558=AXIS2_PLACEMENT_3D('',#17390,#13117,#13118);
#10559=AXIS2_PLACEMENT_3D('',#17392,#13119,#13120);
#10560=AXIS2_PLACEMENT_3D('',#17395,#13122,#13123);
#10561=AXIS2_PLACEMENT_3D('',#17396,#13124,#13125);
#10562=AXIS2_PLACEMENT_3D('',#17398,#13126,#13127);
#10563=AXIS2_PLACEMENT_3D('',#17399,#13128,#13129);
#10564=AXIS2_PLACEMENT_3D('',#17400,#13130,#13131);
#10565=AXIS2_PLACEMENT_3D('',#17402,#13132,#13133);
#10566=AXIS2_PLACEMENT_3D('',#17405,#13135,#13136);
#10567=AXIS2_PLACEMENT_3D('',#17406,#13137,#13138);
#10568=AXIS2_PLACEMENT_3D('',#17408,#13139,#13140);
#10569=AXIS2_PLACEMENT_3D('',#17410,#13141,#13142);
#10570=AXIS2_PLACEMENT_3D('',#17411,#13143,#13144);
#10571=AXIS2_PLACEMENT_3D('',#17412,#13145,#13146);
#10572=AXIS2_PLACEMENT_3D('',#17414,#13147,#13148);
#10573=AXIS2_PLACEMENT_3D('',#17415,#13149,#13150);
#10574=AXIS2_PLACEMENT_3D('',#17416,#13151,#13152);
#10575=AXIS2_PLACEMENT_3D('',#17418,#13153,#13154);
#10576=AXIS2_PLACEMENT_3D('',#17420,#13155,#13156);
#10577=AXIS2_PLACEMENT_3D('',#17422,#13157,#13158);
#10578=AXIS2_PLACEMENT_3D('',#17423,#13159,#13160);
#10579=AXIS2_PLACEMENT_3D('',#17424,#13161,#13162);
#10580=AXIS2_PLACEMENT_3D('',#17427,#13163,#13164);
#10581=AXIS2_PLACEMENT_3D('',#17429,#13166,#13167);
#10582=AXIS2_PLACEMENT_3D('',#17430,#13168,#13169);
#10583=AXIS2_PLACEMENT_3D('',#17432,#13170,#13171);
#10584=AXIS2_PLACEMENT_3D('',#17433,#13172,#13173);
#10585=AXIS2_PLACEMENT_3D('',#17434,#13174,#13175);
#10586=AXIS2_PLACEMENT_3D('',#17435,#13176,#13177);
#10587=AXIS2_PLACEMENT_3D('',#17436,#13178,#13179);
#10588=AXIS2_PLACEMENT_3D('',#17437,#13180,#13181);
#10589=AXIS2_PLACEMENT_3D('',#17438,#13182,#13183);
#10590=AXIS2_PLACEMENT_3D('',#17439,#13184,#13185);
#10591=AXIS2_PLACEMENT_3D('',#17440,#13186,#13187);
#10592=AXIS2_PLACEMENT_3D('',#17441,#13188,#13189);
#10593=AXIS2_PLACEMENT_3D('',#17442,#13190,#13191);
#10594=AXIS2_PLACEMENT_3D('',#17444,#13192,#13193);
#10595=AXIS2_PLACEMENT_3D('',#17448,#13195,#13196);
#10596=AXIS2_PLACEMENT_3D('',#17450,#13197,#13198);
#10597=AXIS2_PLACEMENT_3D('',#17452,#13199,#13200);
#10598=AXIS2_PLACEMENT_3D('',#17454,#13201,#13202);
#10599=AXIS2_PLACEMENT_3D('',#17456,#13203,#13204);
#10600=AXIS2_PLACEMENT_3D('',#17457,#13205,#13206);
#10601=AXIS2_PLACEMENT_3D('',#17458,#13207,#13208);
#10602=AXIS2_PLACEMENT_3D('',#17461,#13209,#13210);
#10603=AXIS2_PLACEMENT_3D('',#17464,#13212,#13213);
#10604=AXIS2_PLACEMENT_3D('',#17465,#13214,#13215);
#10605=AXIS2_PLACEMENT_3D('',#17466,#13216,#13217);
#10606=AXIS2_PLACEMENT_3D('',#17469,#13219,#13220);
#10607=AXIS2_PLACEMENT_3D('',#17470,#13221,#13222);
#10608=AXIS2_PLACEMENT_3D('',#17473,#13224,#13225);
#10609=AXIS2_PLACEMENT_3D('',#17474,#13226,#13227);
#10610=AXIS2_PLACEMENT_3D('',#17484,#13228,#13229);
#10611=AXIS2_PLACEMENT_3D('',#17485,#13230,#13231);
#10612=AXIS2_PLACEMENT_3D('',#17488,#13232,#13233);
#10613=AXIS2_PLACEMENT_3D('',#17490,#13234,#13235);
#10614=AXIS2_PLACEMENT_3D('',#17491,#13236,#13237);
#10615=AXIS2_PLACEMENT_3D('',#17493,#13238,#13239);
#10616=AXIS2_PLACEMENT_3D('',#17494,#13240,#13241);
#10617=AXIS2_PLACEMENT_3D('',#17495,#13242,#13243);
#10618=AXIS2_PLACEMENT_3D('',#17503,#13244,#13245);
#10619=AXIS2_PLACEMENT_3D('',#17511,#13246,#13247);
#10620=AXIS2_PLACEMENT_3D('',#17519,#13248,#13249);
#10621=AXIS2_PLACEMENT_3D('',#17527,#13250,#13251);
#10622=AXIS2_PLACEMENT_3D('',#17535,#13252,#13253);
#10623=AXIS2_PLACEMENT_3D('',#17542,#13258,#13259);
#10624=AXIS2_PLACEMENT_3D('',#17547,#13263,#13264);
#10625=AXIS2_PLACEMENT_3D('',#17552,#13268,#13269);
#10626=AXIS2_PLACEMENT_3D('',#17557,#13273,#13274);
#10627=AXIS2_PLACEMENT_3D('',#17562,#13278,#13279);
#10628=AXIS2_PLACEMENT_3D('',#17565,#13282,#13283);
#10629=AXIS2_PLACEMENT_3D('',#17566,#13284,#13285);
#10630=AXIS2_PLACEMENT_3D('',#17567,#13286,#13287);
#10631=AXIS2_PLACEMENT_3D('',#17568,#13288,#13289);
#10632=AXIS2_PLACEMENT_3D('',#17569,#13290,#13291);
#10633=AXIS2_PLACEMENT_3D('',#17570,#13292,#13293);
#10634=AXIS2_PLACEMENT_3D('',#17571,#13294,#13295);
#10635=AXIS2_PLACEMENT_3D('',#17572,#13296,#13297);
#10636=AXIS2_PLACEMENT_3D('',#17573,#13298,#13299);
#10637=AXIS2_PLACEMENT_3D('',#17576,#13300,#13301);
#10638=AXIS2_PLACEMENT_3D('',#17578,#13302,#13303);
#10639=AXIS2_PLACEMENT_3D('',#17580,#13304,#13305);
#10640=AXIS2_PLACEMENT_3D('',#17582,#13306,#13307);
#10641=AXIS2_PLACEMENT_3D('',#17583,#13308,#13309);
#10642=AXIS2_PLACEMENT_3D('',#17584,#13310,#13311);
#10643=AXIS2_PLACEMENT_3D('',#17586,#13312,#13313);
#10644=AXIS2_PLACEMENT_3D('',#17591,#13316,#13317);
#10645=AXIS2_PLACEMENT_3D('',#17593,#13319,#13320);
#10646=AXIS2_PLACEMENT_3D('',#17595,#13321,#13322);
#10647=AXIS2_PLACEMENT_3D('',#17598,#13324,#13325);
#10648=AXIS2_PLACEMENT_3D('',#17599,#13326,#13327);
#10649=AXIS2_PLACEMENT_3D('',#17601,#13328,#13329);
#10650=AXIS2_PLACEMENT_3D('',#17603,#13331,#13332);
#10651=AXIS2_PLACEMENT_3D('',#17605,#13333,#13334);
#10652=AXIS2_PLACEMENT_3D('',#17607,#13335,#13336);
#10653=AXIS2_PLACEMENT_3D('',#17608,#13337,#13338);
#10654=AXIS2_PLACEMENT_3D('',#17609,#13339,#13340);
#10655=AXIS2_PLACEMENT_3D('',#17611,#13341,#13342);
#10656=AXIS2_PLACEMENT_3D('',#17613,#13344,#13345);
#10657=AXIS2_PLACEMENT_3D('',#17615,#13346,#13347);
#10658=AXIS2_PLACEMENT_3D('',#17617,#13349,#13350);
#10659=AXIS2_PLACEMENT_3D('',#17619,#13351,#13352);
#10660=AXIS2_PLACEMENT_3D('',#17620,#13353,#13354);
#10661=AXIS2_PLACEMENT_3D('',#17621,#13355,#13356);
#10662=AXIS2_PLACEMENT_3D('',#17624,#13357,#13358);
#10663=AXIS2_PLACEMENT_3D('',#17625,#13359,#13360);
#10664=AXIS2_PLACEMENT_3D('',#17628,#13362,#13363);
#10665=AXIS2_PLACEMENT_3D('',#17629,#13364,#13365);
#10666=AXIS2_PLACEMENT_3D('',#17632,#13367,#13368);
#10667=AXIS2_PLACEMENT_3D('',#17633,#13369,#13370);
#10668=AXIS2_PLACEMENT_3D('',#17635,#13371,#13372);
#10669=AXIS2_PLACEMENT_3D('',#17637,#13373,#13374);
#10670=AXIS2_PLACEMENT_3D('',#17638,#13375,#13376);
#10671=AXIS2_PLACEMENT_3D('',#17639,#13377,#13378);
#10672=AXIS2_PLACEMENT_3D('',#17641,#13379,#13380);
#10673=AXIS2_PLACEMENT_3D('',#17643,#13382,#13383);
#10674=AXIS2_PLACEMENT_3D('',#17645,#13384,#13385);
#10675=AXIS2_PLACEMENT_3D('',#17647,#13387,#13388);
#10676=AXIS2_PLACEMENT_3D('',#17649,#13390,#13391);
#10677=AXIS2_PLACEMENT_3D('',#17651,#13393,#13394);
#10678=AXIS2_PLACEMENT_3D('',#17652,#13395,#13396);
#10679=AXIS2_PLACEMENT_3D('',#17653,#13397,#13398);
#10680=AXIS2_PLACEMENT_3D('',#17654,#13399,#13400);
#10681=AXIS2_PLACEMENT_3D('',#17655,#13401,#13402);
#10682=AXIS2_PLACEMENT_3D('',#17656,#13403,#13404);
#10683=AXIS2_PLACEMENT_3D('',#17657,#13405,#13406);
#10684=AXIS2_PLACEMENT_3D('',#17658,#13407,#13408);
#10685=AXIS2_PLACEMENT_3D('',#17660,#13409,#13410);
#10686=AXIS2_PLACEMENT_3D('',#17662,#13411,#13412);
#10687=AXIS2_PLACEMENT_3D('',#17663,#13413,#13414);
#10688=AXIS2_PLACEMENT_3D('',#17664,#13415,#13416);
#10689=AXIS2_PLACEMENT_3D('',#17667,#13417,#13418);
#10690=AXIS2_PLACEMENT_3D('',#17668,#13419,#13420);
#10691=AXIS2_PLACEMENT_3D('',#17669,#13421,#13422);
#10692=AXIS2_PLACEMENT_3D('',#17670,#13423,#13424);
#10693=AXIS2_PLACEMENT_3D('',#17672,#13425,#13426);
#10694=AXIS2_PLACEMENT_3D('',#17675,#13428,#13429);
#10695=AXIS2_PLACEMENT_3D('',#17676,#13430,#13431);
#10696=AXIS2_PLACEMENT_3D('',#17678,#13432,#13433);
#10697=AXIS2_PLACEMENT_3D('',#17680,#13434,#13435);
#10698=AXIS2_PLACEMENT_3D('',#17682,#13436,#13437);
#10699=AXIS2_PLACEMENT_3D('',#17683,#13438,#13439);
#10700=AXIS2_PLACEMENT_3D('',#17684,#13440,#13441);
#10701=AXIS2_PLACEMENT_3D('',#17686,#13443,#13444);
#10702=AXIS2_PLACEMENT_3D('',#17688,#13445,#13446);
#10703=AXIS2_PLACEMENT_3D('',#17689,#13447,#13448);
#10704=AXIS2_PLACEMENT_3D('',#17690,#13449,#13450);
#10705=AXIS2_PLACEMENT_3D('',#17692,#13451,#13452);
#10706=AXIS2_PLACEMENT_3D('',#17693,#13453,#13454);
#10707=AXIS2_PLACEMENT_3D('',#17694,#13455,#13456);
#10708=AXIS2_PLACEMENT_3D('',#17696,#13457,#13458);
#10709=AXIS2_PLACEMENT_3D('',#17698,#13459,#13460);
#10710=AXIS2_PLACEMENT_3D('',#17699,#13461,#13462);
#10711=AXIS2_PLACEMENT_3D('',#17700,#13463,#13464);
#10712=AXIS2_PLACEMENT_3D('',#17702,#13465,#13466);
#10713=AXIS2_PLACEMENT_3D('',#17704,#13467,#13468);
#10714=AXIS2_PLACEMENT_3D('',#17705,#13469,#13470);
#10715=AXIS2_PLACEMENT_3D('',#17706,#13471,#13472);
#10716=AXIS2_PLACEMENT_3D('',#17709,#13473,#13474);
#10717=AXIS2_PLACEMENT_3D('',#17711,#13476,#13477);
#10718=AXIS2_PLACEMENT_3D('',#17712,#13478,#13479);
#10719=AXIS2_PLACEMENT_3D('',#17714,#13480,#13481);
#10720=AXIS2_PLACEMENT_3D('',#17715,#13482,#13483);
#10721=AXIS2_PLACEMENT_3D('',#17716,#13484,#13485);
#10722=AXIS2_PLACEMENT_3D('',#17725,#13490,#13491);
#10723=AXIS2_PLACEMENT_3D('',#17731,#13495,#13496);
#10724=AXIS2_PLACEMENT_3D('',#17737,#13500,#13501);
#10725=AXIS2_PLACEMENT_3D('',#17743,#13505,#13506);
#10726=AXIS2_PLACEMENT_3D('',#17749,#13510,#13511);
#10727=AXIS2_PLACEMENT_3D('',#17755,#13515,#13516);
#10728=AXIS2_PLACEMENT_3D('',#17761,#13520,#13521);
#10729=AXIS2_PLACEMENT_3D('',#17764,#13524,#13525);
#10730=AXIS2_PLACEMENT_3D('',#17765,#13526,#13527);
#10731=AXIS2_PLACEMENT_3D('',#17766,#13528,#13529);
#10732=AXIS2_PLACEMENT_3D('',#17767,#13530,#13531);
#10733=AXIS2_PLACEMENT_3D('',#17768,#13532,#13533);
#10734=AXIS2_PLACEMENT_3D('',#17769,#13534,#13535);
#10735=AXIS2_PLACEMENT_3D('',#17771,#13536,#13537);
#10736=AXIS2_PLACEMENT_3D('',#17774,#13539,#13540);
#10737=AXIS2_PLACEMENT_3D('',#17775,#13541,#13542);
#10738=AXIS2_PLACEMENT_3D('',#17777,#13543,#13544);
#10739=AXIS2_PLACEMENT_3D('',#17780,#13546,#13547);
#10740=AXIS2_PLACEMENT_3D('',#17781,#13548,#13549);
#10741=AXIS2_PLACEMENT_3D('',#17783,#13550,#13551);
#10742=AXIS2_PLACEMENT_3D('',#17786,#13553,#13554);
#10743=AXIS2_PLACEMENT_3D('',#17787,#13555,#13556);
#10744=AXIS2_PLACEMENT_3D('',#17789,#13557,#13558);
#10745=AXIS2_PLACEMENT_3D('',#17791,#13559,#13560);
#10746=AXIS2_PLACEMENT_3D('',#17792,#13561,#13562);
#10747=AXIS2_PLACEMENT_3D('',#17793,#13563,#13564);
#10748=AXIS2_PLACEMENT_3D('',#17795,#13565,#13566);
#10749=AXIS2_PLACEMENT_3D('',#17797,#13568,#13569);
#10750=AXIS2_PLACEMENT_3D('',#17799,#13570,#13571);
#10751=AXIS2_PLACEMENT_3D('',#17800,#13572,#13573);
#10752=AXIS2_PLACEMENT_3D('',#17801,#13574,#13575);
#10753=AXIS2_PLACEMENT_3D('',#17803,#13576,#13577);
#10754=AXIS2_PLACEMENT_3D('',#17806,#13579,#13580);
#10755=AXIS2_PLACEMENT_3D('',#17807,#13581,#13582);
#10756=AXIS2_PLACEMENT_3D('',#17809,#13583,#13584);
#10757=AXIS2_PLACEMENT_3D('',#17812,#13586,#13587);
#10758=AXIS2_PLACEMENT_3D('',#17813,#13588,#13589);
#10759=AXIS2_PLACEMENT_3D('',#17815,#13590,#13591);
#10760=AXIS2_PLACEMENT_3D('',#17818,#13593,#13594);
#10761=AXIS2_PLACEMENT_3D('',#17819,#13595,#13596);
#10762=AXIS2_PLACEMENT_3D('',#17821,#13597,#13598);
#10763=AXIS2_PLACEMENT_3D('',#17824,#13600,#13601);
#10764=AXIS2_PLACEMENT_3D('',#17825,#13602,#13603);
#10765=AXIS2_PLACEMENT_3D('',#17826,#13604,#13605);
#10766=AXIS2_PLACEMENT_3D('',#17827,#13606,#13607);
#10767=AXIS2_PLACEMENT_3D('',#17828,#13608,#13609);
#10768=AXIS2_PLACEMENT_3D('',#17829,#13610,#13611);
#10769=AXIS2_PLACEMENT_3D('',#17830,#13612,#13613);
#10770=AXIS2_PLACEMENT_3D('',#17831,#13614,#13615);
#10771=AXIS2_PLACEMENT_3D('',#17832,#13616,#13617);
#10772=AXIS2_PLACEMENT_3D('',#17833,#13618,#13619);
#10773=AXIS2_PLACEMENT_3D('',#17834,#13620,#13621);
#10774=AXIS2_PLACEMENT_3D('',#17836,#13622,#13623);
#10775=AXIS2_PLACEMENT_3D('',#17839,#13625,#13626);
#10776=AXIS2_PLACEMENT_3D('',#17840,#13627,#13628);
#10777=AXIS2_PLACEMENT_3D('',#17842,#13629,#13630);
#10778=AXIS2_PLACEMENT_3D('',#17844,#13631,#13632);
#10779=AXIS2_PLACEMENT_3D('',#17845,#13633,#13634);
#10780=AXIS2_PLACEMENT_3D('',#17846,#13635,#13636);
#10781=AXIS2_PLACEMENT_3D('',#17849,#13638,#13639);
#10782=AXIS2_PLACEMENT_3D('',#17850,#13640,#13641);
#10783=AXIS2_PLACEMENT_3D('',#17852,#13642,#13643);
#10784=AXIS2_PLACEMENT_3D('',#17853,#13644,#13645);
#10785=AXIS2_PLACEMENT_3D('',#17854,#13646,#13647);
#10786=AXIS2_PLACEMENT_3D('',#17856,#13648,#13649);
#10787=AXIS2_PLACEMENT_3D('',#17859,#13651,#13652);
#10788=AXIS2_PLACEMENT_3D('',#17860,#13653,#13654);
#10789=AXIS2_PLACEMENT_3D('',#17862,#13655,#13656);
#10790=AXIS2_PLACEMENT_3D('',#17864,#13657,#13658);
#10791=AXIS2_PLACEMENT_3D('',#17866,#13659,#13660);
#10792=AXIS2_PLACEMENT_3D('',#17867,#13661,#13662);
#10793=AXIS2_PLACEMENT_3D('',#17868,#13663,#13664);
#10794=AXIS2_PLACEMENT_3D('',#17871,#13665,#13666);
#10795=AXIS2_PLACEMENT_3D('',#17873,#13668,#13669);
#10796=AXIS2_PLACEMENT_3D('',#17874,#13670,#13671);
#10797=AXIS2_PLACEMENT_3D('',#17876,#13672,#13673);
#10798=AXIS2_PLACEMENT_3D('',#17878,#13674,#13675);
#10799=AXIS2_PLACEMENT_3D('',#17879,#13676,#13677);
#10800=AXIS2_PLACEMENT_3D('',#17880,#13678,#13679);
#10801=AXIS2_PLACEMENT_3D('',#17883,#13680,#13681);
#10802=AXIS2_PLACEMENT_3D('',#17885,#13683,#13684);
#10803=AXIS2_PLACEMENT_3D('',#17886,#13685,#13686);
#10804=AXIS2_PLACEMENT_3D('',#17889,#13688,#13689);
#10805=AXIS2_PLACEMENT_3D('',#17890,#13690,#13691);
#10806=AXIS2_PLACEMENT_3D('',#17892,#13692,#13693);
#10807=AXIS2_PLACEMENT_3D('',#17893,#13694,#13695);
#10808=AXIS2_PLACEMENT_3D('',#17894,#13696,#13697);
#10809=AXIS2_PLACEMENT_3D('',#17897,#13699,#13700);
#10810=AXIS2_PLACEMENT_3D('',#17898,#13701,#13702);
#10811=AXIS2_PLACEMENT_3D('',#17900,#13703,#13704);
#10812=AXIS2_PLACEMENT_3D('',#17901,#13705,#13706);
#10813=AXIS2_PLACEMENT_3D('',#17902,#13707,#13708);
#10814=AXIS2_PLACEMENT_3D('',#17903,#13709,#13710);
#10815=AXIS2_PLACEMENT_3D('',#17904,#13711,#13712);
#10816=AXIS2_PLACEMENT_3D('',#17905,#13713,#13714);
#10817=AXIS2_PLACEMENT_3D('',#17906,#13715,#13716);
#10818=AXIS2_PLACEMENT_3D('',#17907,#13717,#13718);
#10819=AXIS2_PLACEMENT_3D('',#17909,#13719,#13720);
#10820=AXIS2_PLACEMENT_3D('',#17912,#13722,#13723);
#10821=AXIS2_PLACEMENT_3D('',#17913,#13724,#13725);
#10822=AXIS2_PLACEMENT_3D('',#17915,#13726,#13727);
#10823=AXIS2_PLACEMENT_3D('',#17918,#13729,#13730);
#10824=AXIS2_PLACEMENT_3D('',#17919,#13731,#13732);
#10825=AXIS2_PLACEMENT_3D('',#17920,#13733,#13734);
#10826=AXIS2_PLACEMENT_3D('',#17921,#13735,#13736);
#10827=AXIS2_PLACEMENT_3D('',#17922,#13737,#13738);
#10828=AXIS2_PLACEMENT_3D('',#17925,#13739,#13740);
#10829=AXIS2_PLACEMENT_3D('',#17928,#13742,#13743);
#10830=AXIS2_PLACEMENT_3D('',#17929,#13744,#13745);
#10831=AXIS2_PLACEMENT_3D('',#17930,#13746,#13747);
#10832=AXIS2_PLACEMENT_3D('',#17933,#13749,#13750);
#10833=AXIS2_PLACEMENT_3D('',#17934,#13751,#13752);
#10834=AXIS2_PLACEMENT_3D('',#17937,#13754,#13755);
#10835=AXIS2_PLACEMENT_3D('',#17938,#13756,#13757);
#10836=AXIS2_PLACEMENT_3D('',#17940,#13758,#13759);
#10837=AXIS2_PLACEMENT_3D('',#17943,#13761,#13762);
#10838=AXIS2_PLACEMENT_3D('',#17944,#13763,#13764);
#10839=AXIS2_PLACEMENT_3D('',#17945,#13765,#13766);
#10840=AXIS2_PLACEMENT_3D('',#17946,#13767,#13768);
#10841=AXIS2_PLACEMENT_3D('',#17947,#13769,#13770);
#10842=AXIS2_PLACEMENT_3D('',#17948,#13771,#13772);
#10843=AXIS2_PLACEMENT_3D('',#17949,#13773,#13774);
#10844=AXIS2_PLACEMENT_3D('',#17950,#13775,#13776);
#10845=AXIS2_PLACEMENT_3D('',#17951,#13777,#13778);
#10846=AXIS2_PLACEMENT_3D('',#17952,#13779,#13780);
#10847=AXIS2_PLACEMENT_3D('',#17953,#13781,#13782);
#10848=AXIS2_PLACEMENT_3D('',#17954,#13783,#13784);
#10849=AXIS2_PLACEMENT_3D('',#17955,#13785,#13786);
#10850=AXIS2_PLACEMENT_3D('',#17956,#13787,#13788);
#10851=AXIS2_PLACEMENT_3D('',#17957,#13789,#13790);
#10852=AXIS2_PLACEMENT_3D('',#17958,#13791,#13792);
#10853=AXIS2_PLACEMENT_3D('',#17959,#13793,#13794);
#10854=AXIS2_PLACEMENT_3D('',#17960,#13795,#13796);
#10855=AXIS2_PLACEMENT_3D('',#17961,#13797,#13798);
#10856=AXIS2_PLACEMENT_3D('',#17962,#13799,#13800);
#10857=AXIS2_PLACEMENT_3D('',#17963,#13801,#13802);
#10858=AXIS2_PLACEMENT_3D('',#17964,#13803,#13804);
#10859=AXIS2_PLACEMENT_3D('',#17965,#13805,#13806);
#10860=AXIS2_PLACEMENT_3D('',#17966,#13807,#13808);
#10861=DIRECTION('axis',(0.,0.,1.));
#10862=DIRECTION('refdir',(1.,0.,0.));
#10863=DIRECTION('axis',(0.,0.,1.));
#10864=DIRECTION('refdir',(1.,0.,0.));
#10865=DIRECTION('center_axis',(1.,3.89551938464967E-15,6.32781493568956E-31));
#10866=DIRECTION('ref_axis',(-3.89551938464967E-15,1.,8.11109567411167E-62));
#10867=DIRECTION('center_axis',(-1.,-3.89551938464967E-15,-6.32181852599599E-31));
#10868=DIRECTION('ref_axis',(3.89551938464967E-15,-1.,2.46267666142548E-45));
#10869=DIRECTION('',(1.,3.89551938464967E-15,6.32781493568956E-31));
#10870=DIRECTION('center_axis',(1.,3.89551938464967E-15,6.32781493568956E-31));
#10871=DIRECTION('ref_axis',(-3.89551938464967E-15,1.,-2.46501257444544E-45));
#10872=DIRECTION('center_axis',(1.,3.89551938464967E-15,6.32781493568956E-31));
#10873=DIRECTION('ref_axis',(-3.89551938464967E-15,1.,-4.58615050165474E-60));
#10874=DIRECTION('center_axis',(-1.,-3.89551938464967E-15,-6.32181852599599E-31));
#10875=DIRECTION('ref_axis',(3.89551938464967E-15,-1.,2.46267666142548E-45));
#10876=DIRECTION('',(1.,3.89551938464967E-15,6.32781493568956E-31));
#10877=DIRECTION('center_axis',(1.,3.89551938464967E-15,6.32781493568956E-31));
#10878=DIRECTION('ref_axis',(-3.89551938464967E-15,1.,-2.46501257444544E-45));
#10879=DIRECTION('center_axis',(1.,3.89551938464967E-15,6.32781493568956E-31));
#10880=DIRECTION('ref_axis',(-3.89551938464967E-15,1.,8.11109567411167E-62));
#10881=DIRECTION('center_axis',(1.,3.89551938464967E-15,6.32781493568956E-31));
#10882=DIRECTION('ref_axis',(-3.89551938464967E-15,1.,1.11134276064131E-61));
#10883=DIRECTION('',(1.,3.89551938464967E-15,6.32781493568956E-31));
#10884=DIRECTION('center_axis',(1.,-3.49148133884313E-15,-5.66612798746291E-31));
#10885=DIRECTION('ref_axis',(3.49148133884313E-15,1.,-1.24849656241355E-47));
#10886=DIRECTION('center_axis',(1.,3.89551938464967E-15,6.32781493568956E-31));
#10887=DIRECTION('ref_axis',(-3.89551938464967E-15,1.,-4.58615050165474E-60));
#10888=DIRECTION('center_axis',(1.,3.89551938464967E-15,6.32781493568956E-31));
#10889=DIRECTION('ref_axis',(-3.89551938464967E-15,1.,-4.55612718233173E-60));
#10890=DIRECTION('',(1.,3.89551938464967E-15,6.32781493568956E-31));
#10891=DIRECTION('center_axis',(1.,-3.49148133884313E-15,-5.66612798746291E-31));
#10892=DIRECTION('ref_axis',(3.49148133884313E-15,1.,-1.24849656241308E-47));
#10893=DIRECTION('center_axis',(0.,-1.,-1.22464679914735E-16));
#10894=DIRECTION('ref_axis',(0.,1.22464679914735E-16,-1.));
#10895=DIRECTION('center_axis',(0.,-1.,-1.22464679914735E-16));
#10896=DIRECTION('ref_axis',(0.,1.22464679914735E-16,-1.));
#10897=DIRECTION('',(0.,-1.,-1.22464679914735E-16));
#10898=DIRECTION('center_axis',(0.,-1.,-1.22464679914735E-16));
#10899=DIRECTION('ref_axis',(0.,1.22464679914735E-16,-1.));
#10900=DIRECTION('center_axis',(0.,-1.,-1.22464679914735E-16));
#10901=DIRECTION('ref_axis',(0.,1.22464679914735E-16,-1.));
#10902=DIRECTION('center_axis',(0.,-1.,-1.22464679914735E-16));
#10903=DIRECTION('ref_axis',(0.,1.22464679914735E-16,-1.));
#10904=DIRECTION('',(0.,-1.,-1.22464679914735E-16));
#10905=DIRECTION('center_axis',(0.,-1.,-1.22464679914735E-16));
#10906=DIRECTION('ref_axis',(0.,1.22464679914735E-16,-1.));
#10907=DIRECTION('center_axis',(0.,-1.,-1.22464679914735E-16));
#10908=DIRECTION('ref_axis',(0.,1.22464679914735E-16,-1.));
#10909=DIRECTION('center_axis',(0.,-1.,0.));
#10910=DIRECTION('ref_axis',(0.,0.,-1.));
#10911=DIRECTION('',(0.,-1.,-1.22464679914735E-16));
#10912=DIRECTION('center_axis',(0.,-1.,-1.22464679914735E-16));
#10913=DIRECTION('ref_axis',(0.,1.22464679914735E-16,-1.));
#10914=DIRECTION('center_axis',(0.,-1.,0.));
#10915=DIRECTION('ref_axis',(0.,0.,-1.));
#10916=DIRECTION('center_axis',(0.,-1.,-1.22464679914735E-16));
#10917=DIRECTION('ref_axis',(0.,1.22464679914735E-16,-1.));
#10918=DIRECTION('',(0.,-1.,0.));
#10919=DIRECTION('center_axis',(0.,-1.,0.));
#10920=DIRECTION('ref_axis',(0.,0.,1.));
#10921=DIRECTION('center_axis',(0.,-1.,0.));
#10922=DIRECTION('ref_axis',(0.,0.,-1.));
#10923=DIRECTION('center_axis',(0.,-1.,-1.22464679914735E-16));
#10924=DIRECTION('ref_axis',(0.,1.22464679914735E-16,-1.));
#10925=DIRECTION('',(0.,-1.,0.));
#10926=DIRECTION('center_axis',(0.,-1.,0.));
#10927=DIRECTION('ref_axis',(0.,0.,-1.));
#10928=DIRECTION('center_axis',(0.,-1.,0.));
#10929=DIRECTION('ref_axis',(0.,0.,-1.));
#10930=DIRECTION('center_axis',(0.,-1.,0.));
#10931=DIRECTION('ref_axis',(0.,0.,-1.));
#10932=DIRECTION('',(0.,-1.,0.));
#10933=DIRECTION('center_axis',(0.,-1.,0.));
#10934=DIRECTION('ref_axis',(0.,0.,1.));
#10935=DIRECTION('center_axis',(0.,-1.,0.));
#10936=DIRECTION('ref_axis',(0.,0.,-1.));
#10937=DIRECTION('center_axis',(0.,-1.,0.));
#10938=DIRECTION('ref_axis',(0.,0.,-1.));
#10939=DIRECTION('',(0.,-1.,0.));
#10940=DIRECTION('center_axis',(0.,-1.,0.));
#10941=DIRECTION('ref_axis',(0.,0.,-1.));
#10942=DIRECTION('center_axis',(1.0842021724855E-15,-6.12323399573677E-17,
1.));
#10943=DIRECTION('ref_axis',(1.,-2.72542236090223E-48,-1.0842021724855E-15));
#10944=DIRECTION('',(1.,0.,-1.08420217248551E-15));
#10945=DIRECTION('center_axis',(0.,0.,-1.));
#10946=DIRECTION('ref_axis',(-1.,0.,0.));
#10947=DIRECTION('',(1.,0.,0.));
#10948=DIRECTION('',(0.,-1.,-2.89120579329468E-16));
#10949=DIRECTION('center_axis',(-4.24884710452154E-31,6.12323399573677E-17,
-1.));
#10950=DIRECTION('ref_axis',(0.,1.,6.12323399573677E-17));
#10951=DIRECTION('',(-1.,0.,0.));
#10952=DIRECTION('center_axis',(0.,0.,1.));
#10953=DIRECTION('ref_axis',(-1.,0.,0.));
#10954=DIRECTION('',(-1.,-6.93889390390723E-15,0.));
#10955=DIRECTION('',(0.,1.,0.));
#10956=DIRECTION('center_axis',(0.,1.,1.5770213417971E-16));
#10957=DIRECTION('ref_axis',(0.,-1.5770213417971E-16,1.));
#10958=DIRECTION('',(-1.,0.,0.));
#10959=DIRECTION('',(0.,0.,1.));
#10960=DIRECTION('',(-1.,0.,0.));
#10961=DIRECTION('',(0.,0.,-1.));
#10962=DIRECTION('center_axis',(0.,1.,1.5770213417971E-16));
#10963=DIRECTION('ref_axis',(0.,-1.5770213417971E-16,1.));
#10964=DIRECTION('',(0.,0.,1.));
#10965=DIRECTION('',(-1.,0.,0.));
#10966=DIRECTION('',(0.,0.,-1.));
#10967=DIRECTION('',(-1.,0.,0.));
#10968=DIRECTION('center_axis',(-4.24884710452153E-31,6.12323399573677E-17,
-1.));
#10969=DIRECTION('ref_axis',(0.,1.,6.12323399573677E-17));
#10970=DIRECTION('',(-1.,0.,0.));
#10971=DIRECTION('center_axis',(0.,0.,1.));
#10972=DIRECTION('ref_axis',(1.,0.,0.));
#10973=DIRECTION('',(-1.,0.,0.));
#10974=DIRECTION('',(0.,-1.,0.));
#10975=DIRECTION('center_axis',(8.67361737988404E-16,-6.12323399573677E-17,
1.));
#10976=DIRECTION('ref_axis',(1.,5.37018253511908E-48,-8.67361737988404E-16));
#10977=DIRECTION('',(-1.,0.,0.));
#10978=DIRECTION('center_axis',(0.,0.,-1.));
#10979=DIRECTION('ref_axis',(1.,-2.42861286636753E-14,0.));
#10980=DIRECTION('',(-1.,0.,0.));
#10981=DIRECTION('',(0.,1.,2.89120579329468E-16));
#10982=DIRECTION('center_axis',(1.,0.,0.));
#10983=DIRECTION('ref_axis',(0.,0.,-1.));
#10984=DIRECTION('',(0.,0.,-1.));
#10985=DIRECTION('center_axis',(-1.,0.,0.));
#10986=DIRECTION('ref_axis',(0.,0.,-1.));
#10987=DIRECTION('',(0.,-1.,0.));
#10988=DIRECTION('center_axis',(-1.,0.,0.));
#10989=DIRECTION('ref_axis',(0.,0.,-1.));
#10990=DIRECTION('center_axis',(1.,0.,0.));
#10991=DIRECTION('ref_axis',(0.,0.,-1.));
#10992=DIRECTION('',(0.,1.,0.));
#10993=DIRECTION('',(0.,1.,0.));
#10994=DIRECTION('',(0.,0.,1.));
#10995=DIRECTION('center_axis',(-1.,0.,0.));
#10996=DIRECTION('ref_axis',(0.,0.,1.));
#10997=DIRECTION('',(0.,1.,0.));
#10998=DIRECTION('center_axis',(-1.,0.,0.));
#10999=DIRECTION('ref_axis',(0.,0.,-1.));
#11000=DIRECTION('',(0.,0.,1.));
#11001=DIRECTION('center_axis',(-1.,0.,0.));
#11002=DIRECTION('ref_axis',(0.,0.,-1.));
#11003=DIRECTION('center_axis',(-1.,0.,0.));
#11004=DIRECTION('ref_axis',(0.,0.,1.));
#11005=DIRECTION('',(0.,0.,1.));
#11006=DIRECTION('',(0.,0.,1.));
#11007=DIRECTION('',(0.,-1.,0.));
#11008=DIRECTION('center_axis',(1.,0.,0.));
#11009=DIRECTION('ref_axis',(0.,0.,-1.));
#11010=DIRECTION('',(0.,-0.889029388585715,-0.457850135121645));
#11011=DIRECTION('center_axis',(-1.,0.,0.));
#11012=DIRECTION('ref_axis',(0.,-6.93889390390722E-15,-1.));
#11013=DIRECTION('center_axis',(-1.,0.,0.));
#11014=DIRECTION('ref_axis',(0.,-2.08166817117217E-14,-1.));
#11015=DIRECTION('center_axis',(1.,0.,0.));
#11016=DIRECTION('ref_axis',(0.,0.,-1.));
#11017=DIRECTION('',(0.,0.457850135121644,-0.889029388585716));
#11018=DIRECTION('',(0.,0.457850135121643,-0.889029388585717));
#11019=DIRECTION('',(0.,0.889029388585714,0.457850135121648));
#11020=DIRECTION('center_axis',(-1.,0.,0.));
#11021=DIRECTION('ref_axis',(0.,0.,1.));
#11022=DIRECTION('',(0.,0.,-1.));
#11023=DIRECTION('center_axis',(-1.,0.,0.));
#11024=DIRECTION('ref_axis',(0.,-6.93889390390722E-15,-1.));
#11025=DIRECTION('',(0.,0.889029388585715,0.457850135121645));
#11026=DIRECTION('center_axis',(-1.,0.,0.));
#11027=DIRECTION('ref_axis',(0.,-2.08166817117217E-14,-1.));
#11028=DIRECTION('center_axis',(-1.,0.,0.));
#11029=DIRECTION('ref_axis',(0.,0.,1.));
#11030=DIRECTION('',(0.,1.,0.));
#11031=DIRECTION('',(0.,1.,0.));
#11032=DIRECTION('center_axis',(1.,0.,0.));
#11033=DIRECTION('ref_axis',(0.,0.,-1.));
#11034=DIRECTION('center_axis',(-1.,0.,0.));
#11035=DIRECTION('ref_axis',(0.,1.73472347597681E-14,-1.));
#11036=DIRECTION('center_axis',(-1.,0.,0.));
#11037=DIRECTION('ref_axis',(0.,0.,-1.));
#11038=DIRECTION('center_axis',(-1.,0.,0.));
#11039=DIRECTION('ref_axis',(0.,0.,1.));
#11040=DIRECTION('',(0.,-0.889029388585714,-0.457850135121648));
#11041=DIRECTION('center_axis',(-1.,0.,0.));
#11042=DIRECTION('ref_axis',(0.,1.73472347597681E-14,-1.));
#11043=DIRECTION('center_axis',(-1.,0.,0.));
#11044=DIRECTION('ref_axis',(0.,0.,-1.));
#11045=DIRECTION('center_axis',(-1.,0.,0.));
#11046=DIRECTION('ref_axis',(0.,0.,1.));
#11047=DIRECTION('',(0.,0.457850135121644,-0.889029388585716));
#11048=DIRECTION('',(0.,0.457850135121643,-0.889029388585717));
#11049=DIRECTION('center_axis',(1.,0.,0.));
#11050=DIRECTION('ref_axis',(0.,0.,-1.));
#11051=DIRECTION('',(0.,0.,1.));
#11052=DIRECTION('center_axis',(-1.,0.,0.));
#11053=DIRECTION('ref_axis',(0.,0.,-1.));
#11054=DIRECTION('center_axis',(-1.,0.,0.));
#11055=DIRECTION('ref_axis',(0.,0.,-1.));
#11056=DIRECTION('center_axis',(1.,0.,0.));
#11057=DIRECTION('ref_axis',(0.,0.,-1.));
#11058=DIRECTION('',(0.,-1.,0.));
#11059=DIRECTION('',(0.,-1.,0.));
#11060=DIRECTION('',(0.,0.,-1.));
#11061=DIRECTION('center_axis',(-1.,0.,0.));
#11062=DIRECTION('ref_axis',(0.,0.,1.));
#11063=DIRECTION('center_axis',(-1.,0.,0.));
#11064=DIRECTION('ref_axis',(0.,0.,-1.));
#11065=DIRECTION('',(0.,0.,-1.));
#11066=DIRECTION('center_axis',(-1.,0.,0.));
#11067=DIRECTION('ref_axis',(0.,0.,-1.));
#11068=DIRECTION('center_axis',(1.,0.,0.));
#11069=DIRECTION('ref_axis',(0.,0.,-1.));
#11070=DIRECTION('',(0.,1.,0.));
#11071=DIRECTION('center_axis',(-1.,0.,0.));
#11072=DIRECTION('ref_axis',(0.,0.,-1.));
#11073=DIRECTION('center_axis',(-1.,0.,0.));
#11074=DIRECTION('ref_axis',(0.,0.,-1.));
#11075=DIRECTION('center_axis',(1.,0.,0.));
#11076=DIRECTION('ref_axis',(0.,0.,-1.));
#11077=DIRECTION('',(0.,-1.22464679914735E-16,1.));
#11078=DIRECTION('',(0.,-1.22464679914735E-16,1.));
#11079=DIRECTION('',(0.,1.,0.));
#11080=DIRECTION('center_axis',(-1.,0.,0.));
#11081=DIRECTION('ref_axis',(0.,0.,1.));
#11082=DIRECTION('',(0.,0.,1.));
#11083=DIRECTION('center_axis',(-1.,0.,0.));
#11084=DIRECTION('ref_axis',(0.,0.,-1.));
#11085=DIRECTION('',(0.,-1.,0.));
#11086=DIRECTION('center_axis',(-1.,0.,0.));
#11087=DIRECTION('ref_axis',(0.,0.,-1.));
#11088=DIRECTION('center_axis',(-1.,0.,0.));
#11089=DIRECTION('ref_axis',(0.,0.,1.));
#11090=DIRECTION('',(0.,-1.,0.));
#11091=DIRECTION('',(0.,-1.,0.));
#11092=DIRECTION('center_axis',(0.,-1.,-1.22464679914735E-16));
#11093=DIRECTION('ref_axis',(0.,1.22464679914735E-16,-1.));
#11094=DIRECTION('',(0.,-1.22464679914735E-16,1.));
#11095=DIRECTION('',(-1.,0.,0.));
#11096=DIRECTION('',(-1.,0.,0.));
#11097=DIRECTION('center_axis',(0.,0.,1.));
#11098=DIRECTION('ref_axis',(1.,0.,0.));
#11099=DIRECTION('',(0.,1.,0.));
#11100=DIRECTION('',(-1.,0.,0.));
#11101=DIRECTION('center_axis',(0.,-1.,-1.22464679914735E-16));
#11102=DIRECTION('ref_axis',(0.,1.22464679914735E-16,-1.));
#11103=DIRECTION('',(0.,-1.22464679914735E-16,1.));
#11104=DIRECTION('',(-1.,0.,0.));
#11105=DIRECTION('center_axis',(-1.,0.,0.));
#11106=DIRECTION('ref_axis',(0.,0.,1.));
#11107=DIRECTION('',(-1.,0.,0.));
#11108=DIRECTION('center_axis',(0.,0.,-1.));
#11109=DIRECTION('ref_axis',(-1.,0.,0.));
#11110=DIRECTION('',(-1.,0.,0.));
#11111=DIRECTION('center_axis',(-1.,0.,0.));
#11112=DIRECTION('ref_axis',(0.,0.,1.));
#11113=DIRECTION('center_axis',(-1.,0.,0.));
#11114=DIRECTION('ref_axis',(0.,0.,1.));
#11115=DIRECTION('',(-1.,0.,0.));
#11116=DIRECTION('center_axis',(0.,0.889029388585716,0.457850135121643));
#11117=DIRECTION('ref_axis',(0.,-0.457850135121643,0.889029388585716));
#11118=DIRECTION('',(-1.,0.,0.));
#11119=DIRECTION('center_axis',(-1.,0.,0.));
#11120=DIRECTION('ref_axis',(0.,0.,1.));
#11121=DIRECTION('',(-1.,0.,0.));
#11122=DIRECTION('center_axis',(0.,0.,1.));
#11123=DIRECTION('ref_axis',(1.,0.,0.));
#11124=DIRECTION('',(-1.,0.,0.));
#11125=DIRECTION('center_axis',(-1.,0.,0.));
#11126=DIRECTION('ref_axis',(0.,0.,1.));
#11127=DIRECTION('',(-1.,0.,0.));
#11128=DIRECTION('center_axis',(0.,-1.,0.));
#11129=DIRECTION('ref_axis',(0.,0.,-1.));
#11130=DIRECTION('',(-1.,0.,0.));
#11131=DIRECTION('',(0.,0.,1.));
#11132=DIRECTION('center_axis',(0.,0.,-1.));
#11133=DIRECTION('ref_axis',(-1.,0.,0.));
#11134=DIRECTION('',(-1.,0.,0.));
#11135=DIRECTION('',(0.,-1.,0.));
#11136=DIRECTION('center_axis',(0.,-1.,0.));
#11137=DIRECTION('ref_axis',(0.,0.,-1.));
#11138=DIRECTION('',(-1.,0.,0.));
#11139=DIRECTION('',(0.,0.,1.));
#11140=DIRECTION('center_axis',(-1.,0.,0.));
#11141=DIRECTION('ref_axis',(0.,0.,1.));
#11142=DIRECTION('',(-1.,0.,0.));
#11143=DIRECTION('center_axis',(0.,0.,1.));
#11144=DIRECTION('ref_axis',(1.,0.,0.));
#11145=DIRECTION('',(-1.,0.,0.));
#11146=DIRECTION('center_axis',(-1.,0.,0.));
#11147=DIRECTION('ref_axis',(0.,0.,1.));
#11148=DIRECTION('',(-1.,0.,0.));
#11149=DIRECTION('center_axis',(0.,0.889029388585716,0.457850135121643));
#11150=DIRECTION('ref_axis',(0.,-0.457850135121644,0.889029388585716));
#11151=DIRECTION('',(-1.,0.,0.));
#11152=DIRECTION('center_axis',(-1.,0.,0.));
#11153=DIRECTION('ref_axis',(0.,0.,1.));
#11154=DIRECTION('',(-1.,-6.93889390390723E-15,0.));
#11155=DIRECTION('',(-1.,0.,0.));
#11156=DIRECTION('center_axis',(-1.,0.,0.));
#11157=DIRECTION('ref_axis',(0.,0.,1.));
#11158=DIRECTION('',(-1.,0.,0.));
#11159=DIRECTION('',(-1.,0.,0.));
#11160=DIRECTION('',(1.,0.,-1.08420217248551E-15));
#11161=DIRECTION('center_axis',(0.,0.,-1.));
#11162=DIRECTION('ref_axis',(-1.,0.,0.));
#11163=DIRECTION('',(-1.,0.,0.));
#11164=DIRECTION('center_axis',(-1.,0.,0.));
#11165=DIRECTION('ref_axis',(0.,0.,1.));
#11166=DIRECTION('center_axis',(1.,0.,0.));
#11167=DIRECTION('ref_axis',(0.,0.,-1.));
#11168=DIRECTION('center_axis',(1.,0.,0.));
#11169=DIRECTION('ref_axis',(0.,0.,-1.));
#11170=DIRECTION('center_axis',(0.,0.,-1.));
#11171=DIRECTION('ref_axis',(-1.,0.,0.));
#11172=DIRECTION('center_axis',(0.,0.,-1.));
#11173=DIRECTION('ref_axis',(1.,1.76941794549634E-13,0.));
#11174=DIRECTION('',(1.,3.89551938464967E-15,6.46539339818476E-31));
#11175=DIRECTION('center_axis',(0.,0.,-1.));
#11176=DIRECTION('ref_axis',(1.,0.,0.));
#11177=DIRECTION('center_axis',(0.,0.,-1.));
#11178=DIRECTION('ref_axis',(-1.,0.,0.));
#11179=DIRECTION('center_axis',(0.,0.,1.));
#11180=DIRECTION('ref_axis',(1.,0.,0.));
#11181=DIRECTION('center_axis',(0.,0.,1.));
#11182=DIRECTION('ref_axis',(1.,0.,0.));
#11183=DIRECTION('',(1.,3.89551938464967E-15,5.66612798746291E-31));
#11184=DIRECTION('center_axis',(0.,0.,1.));
#11185=DIRECTION('ref_axis',(1.,3.46944695195361E-15,0.));
#11186=DIRECTION('',(6.32181852599599E-31,2.46267666142548E-45,-1.));
#11187=DIRECTION('center_axis',(0.,0.,1.));
#11188=DIRECTION('ref_axis',(1.,0.,0.));
#11189=DIRECTION('',(-6.32181852599599E-31,-2.46267666142548E-45,1.));
#11190=DIRECTION('center_axis',(5.66612798746291E-31,2.20725114110678E-45,
-1.));
#11191=DIRECTION('ref_axis',(-1.,1.16909086576945E-91,-5.66612798746291E-31));
#11192=DIRECTION('',(3.89551938464967E-15,-1.,0.));
#11193=DIRECTION('',(1.,3.89551938464967E-15,6.32781493568956E-31));
#11194=DIRECTION('',(3.89551938464967E-15,-1.,0.));
#11195=DIRECTION('center_axis',(1.24069748425108E-31,-1.97819343751741E-16,
1.));
#11196=DIRECTION('ref_axis',(0.,-1.,-1.97819343751741E-16));
#11197=DIRECTION('',(-3.89551938464967E-15,1.,1.97819343751741E-16));
#11198=DIRECTION('',(-1.,-3.49148133884313E-15,-5.66612798746291E-31));
#11199=DIRECTION('',(-3.89551938464967E-15,1.,1.97819343751741E-16));
#11200=DIRECTION('center_axis',(-1.,-3.89551938464967E-15,-6.32181852599599E-31));
#11201=DIRECTION('ref_axis',(3.89551938464967E-15,-1.,3.65599846003365E-62));
#11202=DIRECTION('',(1.84901925624628E-15,-0.450343689478977,0.892855285780659));
#11203=DIRECTION('',(4.27488727659472E-15,-1.,0.));
#11204=DIRECTION('',(8.75811540203011E-47,1.62284355480483E-16,-1.));
#11205=DIRECTION('center_axis',(-1.,-3.89551938464967E-15,-6.32181852599599E-31));
#11206=DIRECTION('ref_axis',(3.89551938464967E-15,-1.,3.65599846003365E-62));
#11207=DIRECTION('',(8.75811540203011E-47,1.62284355480483E-16,-1.));
#11208=DIRECTION('',(4.27488727659472E-15,-1.,0.));
#11209=DIRECTION('',(1.84901925624628E-15,-0.450343689478977,0.892855285780659));
#11210=DIRECTION('center_axis',(-3.49148133884313E-15,1.,1.62284355480483E-16));
#11211=DIRECTION('ref_axis',(-1.,-3.49148133884313E-15,0.));
#11212=DIRECTION('',(1.,3.89551938464967E-15,6.32781493568956E-31));
#11213=DIRECTION('center_axis',(-6.32781493568956E-31,-2.70506955572254E-45,
1.));
#11214=DIRECTION('ref_axis',(1.,-7.97759856789153E-92,6.32781493568956E-31));
#11215=DIRECTION('',(1.,3.89551938464967E-15,6.32781493568956E-31));
#11216=DIRECTION('center_axis',(-3.47813507344548E-15,0.892855285780659,
0.450343689478978));
#11217=DIRECTION('ref_axis',(5.27827569634311E-32,-0.450343689478977,0.892855285780659));
#11218=DIRECTION('center_axis',(0.,0.,1.));
#11219=DIRECTION('ref_axis',(1.,0.,0.));
#11220=DIRECTION('center_axis',(0.,0.,1.));
#11221=DIRECTION('ref_axis',(-1.,0.,0.));
#11222=DIRECTION('center_axis',(0.,0.,1.));
#11223=DIRECTION('ref_axis',(-1.,3.46944695195361E-15,0.));
#11224=DIRECTION('',(-1.,3.49148133884313E-15,5.66612798746291E-31));
#11225=DIRECTION('center_axis',(0.,0.,1.));
#11226=DIRECTION('ref_axis',(1.,0.,0.));
#11227=DIRECTION('center_axis',(0.,0.,-1.));
#11228=DIRECTION('ref_axis',(-1.,0.,0.));
#11229=DIRECTION('center_axis',(0.,0.,-1.));
#11230=DIRECTION('ref_axis',(-1.,0.,0.));
#11231=DIRECTION('',(-1.,3.49148133884313E-15,5.66612798746291E-31));
#11232=DIRECTION('center_axis',(0.,0.,-1.));
#11233=DIRECTION('ref_axis',(-1.,3.46944695195361E-15,0.));
#11234=DIRECTION('',(0.,-1.62284355480483E-16,1.));
#11235=DIRECTION('center_axis',(0.,0.,-1.));
#11236=DIRECTION('ref_axis',(-1.,0.,0.));
#11237=DIRECTION('',(0.,1.62284355480483E-16,-1.));
#11238=DIRECTION('center_axis',(-5.66612798746291E-31,1.97831801317236E-45,
-1.));
#11239=DIRECTION('ref_axis',(-1.,3.87718526908309E-92,5.66612798746291E-31));
#11240=DIRECTION('',(3.49148133884313E-15,1.,0.));
#11241=DIRECTION('',(-1.,3.49148133884313E-15,5.6715024575856E-31));
#11242=DIRECTION('',(3.49148133884313E-15,1.,0.));
#11243=DIRECTION('center_axis',(-7.61622868891015E-31,-3.80421814907195E-16,
1.));
#11244=DIRECTION('ref_axis',(0.,-1.,-3.80421814907195E-16));
#11245=DIRECTION('',(-3.49148133884313E-15,-1.,-3.80421814907195E-16));
#11246=DIRECTION('',(1.,-3.49148133884313E-15,-5.66612798746291E-31));
#11247=DIRECTION('',(-3.49148133884313E-15,-1.,-3.80421814907195E-16));
#11248=DIRECTION('center_axis',(1.,-3.49148133884313E-15,-5.66612798746291E-31));
#11249=DIRECTION('ref_axis',(3.49148133884313E-15,1.,-3.25324957840726E-62));
#11250=DIRECTION('',(0.,-1.62284355480483E-16,1.));
#11251=DIRECTION('',(3.49148133884313E-15,1.,0.));
#11252=DIRECTION('',(1.57236658788162E-15,0.450343689478977,-0.892855285780659));
#11253=DIRECTION('center_axis',(1.,-3.49148133884313E-15,-5.66612798746291E-31));
#11254=DIRECTION('ref_axis',(3.49148133884313E-15,1.,-3.25324957840726E-62));
#11255=DIRECTION('',(1.57236658788162E-15,0.450343689478977,-0.892855285780659));
#11256=DIRECTION('',(3.49148133884313E-15,1.,0.));
#11257=DIRECTION('',(0.,-1.62284355480483E-16,1.));
#11258=DIRECTION('center_axis',(3.49148133884313E-15,1.,1.62284355480483E-16));
#11259=DIRECTION('ref_axis',(-1.,3.49148133884313E-15,0.));
#11260=DIRECTION('',(-1.,3.49148133884313E-15,5.6715024575856E-31));
#11261=DIRECTION('center_axis',(3.11738756859062E-15,0.892855285780659,
0.450343689478978));
#11262=DIRECTION('ref_axis',(6.19177544941703E-32,-0.450343689478977,0.892855285780659));
#11263=DIRECTION('',(-1.,3.49148133884313E-15,5.6715024575856E-31));
#11264=DIRECTION('center_axis',(5.6715024575856E-31,-1.98019449938631E-45,
1.));
#11265=DIRECTION('ref_axis',(1.,8.02907465960574E-92,-5.6715024575856E-31));
#11266=DIRECTION('axis',(0.,0.,1.));
#11267=DIRECTION('refdir',(1.,0.,0.));
#11268=DIRECTION('center_axis',(0.,0.,1.));
#11269=DIRECTION('ref_axis',(1.,0.,0.));
#11270=DIRECTION('center_axis',(0.,-3.89551938464967E-15,-1.));
#11271=DIRECTION('ref_axis',(0.,1.,-3.89551938464967E-15));
#11272=DIRECTION('',(0.,0.,1.));
#11273=DIRECTION('center_axis',(0.,0.,1.));
#11274=DIRECTION('ref_axis',(1.,0.,0.));
#11275=DIRECTION('center_axis',(0.,0.,1.));
#11276=DIRECTION('ref_axis',(1.,0.,0.));
#11277=DIRECTION('center_axis',(0.,-3.89551938464967E-15,-1.));
#11278=DIRECTION('ref_axis',(0.,1.,-3.89551938464967E-15));
#11279=DIRECTION('',(0.,0.,1.));
#11280=DIRECTION('center_axis',(0.,0.,1.));
#11281=DIRECTION('ref_axis',(1.,0.,0.));
#11282=DIRECTION('center_axis',(0.,0.,1.));
#11283=DIRECTION('ref_axis',(1.,0.,0.));
#11284=DIRECTION('center_axis',(0.,0.,1.));
#11285=DIRECTION('ref_axis',(1.,0.,0.));
#11286=DIRECTION('',(0.,0.,1.));
#11287=DIRECTION('center_axis',(0.,-3.49148133884313E-15,1.));
#11288=DIRECTION('ref_axis',(0.,-1.,-3.49148133884313E-15));
#11289=DIRECTION('center_axis',(0.,0.,1.));
#11290=DIRECTION('ref_axis',(1.,0.,0.));
#11291=DIRECTION('center_axis',(0.,0.,1.));
#11292=DIRECTION('ref_axis',(1.,0.,0.));
#11293=DIRECTION('',(0.,0.,1.));
#11294=DIRECTION('center_axis',(0.,-3.49148133884313E-15,1.));
#11295=DIRECTION('ref_axis',(0.,-1.,-3.49148133884313E-15));
#11296=DIRECTION('center_axis',(0.,-1.,0.));
#11297=DIRECTION('ref_axis',(0.,0.,-1.));
#11298=DIRECTION('center_axis',(1.22464679914735E-16,-1.,0.));
#11299=DIRECTION('ref_axis',(1.,1.22464679914735E-16,0.));
#11300=DIRECTION('',(0.,-1.,0.));
#11301=DIRECTION('center_axis',(0.,-1.,0.));
#11302=DIRECTION('ref_axis',(0.,0.,1.));
#11303=DIRECTION('center_axis',(0.,-1.,0.));
#11304=DIRECTION('ref_axis',(0.,0.,-1.));
#11305=DIRECTION('center_axis',(1.22464679914735E-16,-1.,0.));
#11306=DIRECTION('ref_axis',(1.,1.22464679914735E-16,0.));
#11307=DIRECTION('',(0.,-1.,0.));
#11308=DIRECTION('center_axis',(0.,-1.,0.));
#11309=DIRECTION('ref_axis',(0.,0.,-1.));
#11310=DIRECTION('center_axis',(0.,-1.,0.));
#11311=DIRECTION('ref_axis',(0.,0.,-1.));
#11312=DIRECTION('center_axis',(0.,-1.,0.));
#11313=DIRECTION('ref_axis',(0.,0.,-1.));
#11314=DIRECTION('',(0.,-1.,0.));
#11315=DIRECTION('center_axis',(0.,-1.,0.));
#11316=DIRECTION('ref_axis',(0.,0.,1.));
#11317=DIRECTION('center_axis',(0.,-1.,0.));
#11318=DIRECTION('ref_axis',(0.,0.,-1.));
#11319=DIRECTION('center_axis',(0.,-1.,0.));
#11320=DIRECTION('ref_axis',(0.,0.,-1.));
#11321=DIRECTION('',(0.,-1.,0.));
#11322=DIRECTION('center_axis',(0.,-1.,0.));
#11323=DIRECTION('ref_axis',(0.,0.,-1.));
#11324=DIRECTION('center_axis',(-1.,0.,0.));
#11325=DIRECTION('ref_axis',(0.,0.,1.));
#11326=DIRECTION('',(0.,0.,1.));
#11327=DIRECTION('center_axis',(1.,0.,0.));
#11328=DIRECTION('ref_axis',(0.,0.,-1.));
#11329=DIRECTION('',(0.,0.,1.));
#11330=DIRECTION('',(0.,-1.,0.));
#11331=DIRECTION('center_axis',(1.,5.31105888065192E-32,-8.67361737988404E-16));
#11332=DIRECTION('ref_axis',(-8.67361737988404E-16,0.,-1.));
#11333=DIRECTION('',(0.,0.,-1.));
#11334=DIRECTION('center_axis',(-1.,0.,0.));
#11335=DIRECTION('ref_axis',(0.,0.,-1.));
#11336=DIRECTION('',(-8.67361737988404E-16,0.,-1.));
#11337=DIRECTION('',(0.,1.,0.));
#11338=DIRECTION('center_axis',(0.,1.,0.));
#11339=DIRECTION('ref_axis',(0.,0.,1.));
#11340=DIRECTION('',(0.,0.,-1.));
#11341=DIRECTION('',(-1.,0.,0.));
#11342=DIRECTION('',(0.,0.,-1.));
#11343=DIRECTION('',(1.,0.,0.));
#11344=DIRECTION('center_axis',(0.,1.,0.));
#11345=DIRECTION('ref_axis',(0.,0.,1.));
#11346=DIRECTION('',(-1.,0.,0.));
#11347=DIRECTION('',(0.,0.,-1.));
#11348=DIRECTION('',(1.,0.,0.));
#11349=DIRECTION('',(0.,0.,-1.));
#11350=DIRECTION('center_axis',(1.,-3.98329416048893E-32,6.50521303491302E-16));
#11351=DIRECTION('ref_axis',(6.50521303491302E-16,0.,-1.));
#11352=DIRECTION('',(0.,0.,-1.));
#11353=DIRECTION('center_axis',(-1.,0.,0.));
#11354=DIRECTION('ref_axis',(0.,0.,1.));
#11355=DIRECTION('',(0.,0.,-1.));
#11356=DIRECTION('',(0.,-1.,0.));
#11357=DIRECTION('center_axis',(-1.,0.,0.));
#11358=DIRECTION('ref_axis',(0.,0.,1.));
#11359=DIRECTION('',(0.,0.,-1.));
#11360=DIRECTION('center_axis',(1.,0.,0.));
#11361=DIRECTION('ref_axis',(0.,-2.42861286636753E-14,1.));
#11362=DIRECTION('',(0.,0.,-1.));
#11363=DIRECTION('',(0.,1.,0.));
#11364=DIRECTION('center_axis',(0.,0.,1.));
#11365=DIRECTION('ref_axis',(1.,0.,0.));
#11366=DIRECTION('',(1.,0.,0.));
#11367=DIRECTION('center_axis',(0.,0.,-1.));
#11368=DIRECTION('ref_axis',(1.,0.,0.));
#11369=DIRECTION('',(0.,-1.,0.));
#11370=DIRECTION('center_axis',(0.,0.,-1.));
#11371=DIRECTION('ref_axis',(1.,0.,0.));
#11372=DIRECTION('center_axis',(0.,0.,1.));
#11373=DIRECTION('ref_axis',(1.,0.,0.));
#11374=DIRECTION('',(0.,1.,0.));
#11375=DIRECTION('',(0.,1.,0.));
#11376=DIRECTION('',(-1.,0.,0.));
#11377=DIRECTION('center_axis',(0.,0.,-1.));
#11378=DIRECTION('ref_axis',(-1.,0.,0.));
#11379=DIRECTION('',(0.,1.,0.));
#11380=DIRECTION('center_axis',(0.,0.,-1.));
#11381=DIRECTION('ref_axis',(1.,0.,0.));
#11382=DIRECTION('',(-1.,0.,0.));
#11383=DIRECTION('center_axis',(0.,0.,-1.));
#11384=DIRECTION('ref_axis',(1.,0.,0.));
#11385=DIRECTION('center_axis',(0.,0.,-1.));
#11386=DIRECTION('ref_axis',(-1.,0.,0.));
#11387=DIRECTION('',(-1.,0.,0.));
#11388=DIRECTION('',(-1.,0.,0.));
#11389=DIRECTION('',(0.,-1.,0.));
#11390=DIRECTION('center_axis',(0.,0.,1.));
#11391=DIRECTION('ref_axis',(1.,0.,0.));
#11392=DIRECTION('center_axis',(0.,0.,-1.));
#11393=DIRECTION('ref_axis',(1.,0.,0.));
#11394=DIRECTION('center_axis',(0.,0.,-1.));
#11395=DIRECTION('ref_axis',(1.,0.,0.));
#11396=DIRECTION('center_axis',(0.,0.,-1.));
#11397=DIRECTION('ref_axis',(-1.,0.,0.));
#11398=DIRECTION('',(1.,0.,0.));
#11399=DIRECTION('center_axis',(0.,0.,-1.));
#11400=DIRECTION('ref_axis',(1.,0.,0.));
#11401=DIRECTION('center_axis',(0.,0.,-1.));
#11402=DIRECTION('ref_axis',(1.,0.,0.));
#11403=DIRECTION('center_axis',(0.,0.,-1.));
#11404=DIRECTION('ref_axis',(-1.,0.,0.));
#11405=DIRECTION('',(0.,1.,0.));
#11406=DIRECTION('',(0.,1.,0.));
#11407=DIRECTION('center_axis',(0.,0.,1.));
#11408=DIRECTION('ref_axis',(1.,0.,0.));
#11409=DIRECTION('',(-0.457850135121646,-0.889029388585715,0.));
#11410=DIRECTION('center_axis',(0.,0.,-1.));
#11411=DIRECTION('ref_axis',(1.,3.46944695195361E-15,0.));
#11412=DIRECTION('center_axis',(0.,0.,-1.));
#11413=DIRECTION('ref_axis',(1.,0.,0.));
#11414=DIRECTION('center_axis',(0.,0.,1.));
#11415=DIRECTION('ref_axis',(1.,0.,0.));
#11416=DIRECTION('',(0.889029388585716,-0.457850135121644,0.));
#11417=DIRECTION('',(0.889029388585716,-0.457850135121644,0.));
#11418=DIRECTION('',(0.457850135121646,0.889029388585715,0.));
#11419=DIRECTION('center_axis',(0.,0.,-1.));
#11420=DIRECTION('ref_axis',(-1.,0.,0.));
#11421=DIRECTION('center_axis',(0.,0.,-1.));
#11422=DIRECTION('ref_axis',(1.,3.46944695195361E-15,0.));
#11423=DIRECTION('',(0.457850135121646,0.889029388585715,0.));
#11424=DIRECTION('center_axis',(0.,0.,-1.));
#11425=DIRECTION('ref_axis',(1.,0.,0.));
#11426=DIRECTION('center_axis',(0.,0.,1.));
#11427=DIRECTION('ref_axis',(1.,0.,0.));
#11428=DIRECTION('',(-1.,0.,0.));
#11429=DIRECTION('center_axis',(0.,0.,-1.));
#11430=DIRECTION('ref_axis',(1.,-3.46944695195361E-15,0.));
#11431=DIRECTION('center_axis',(0.,0.,-1.));
#11432=DIRECTION('ref_axis',(1.,0.,0.));
#11433=DIRECTION('center_axis',(0.,0.,1.));
#11434=DIRECTION('ref_axis',(1.,0.,0.));
#11435=DIRECTION('',(0.,-1.,0.));
#11436=DIRECTION('',(0.,-1.,0.));
#11437=DIRECTION('',(1.,6.64977332457776E-15,0.));
#11438=DIRECTION('center_axis',(0.,0.,-1.));
#11439=DIRECTION('ref_axis',(-1.,0.,0.));
#11440=DIRECTION('',(-0.457850135121646,-0.889029388585715,0.));
#11441=DIRECTION('center_axis',(0.,0.,-1.));
#11442=DIRECTION('ref_axis',(1.,-3.46944695195361E-15,0.));
#11443=DIRECTION('',(1.,0.,0.));
#11444=DIRECTION('center_axis',(0.,0.,-1.));
#11445=DIRECTION('ref_axis',(1.,0.,0.));
#11446=DIRECTION('center_axis',(0.,0.,-1.));
#11447=DIRECTION('ref_axis',(-1.,0.,0.));
#11448=DIRECTION('',(0.889029388585716,-0.457850135121644,0.));
#11449=DIRECTION('',(0.889029388585716,-0.457850135121644,0.));
#11450=DIRECTION('center_axis',(0.,0.,1.));
#11451=DIRECTION('ref_axis',(1.,0.,0.));
#11452=DIRECTION('',(0.,1.,0.));
#11453=DIRECTION('center_axis',(0.,0.,-1.));
#11454=DIRECTION('ref_axis',(1.,0.,0.));
#11455=DIRECTION('center_axis',(0.,0.,-1.));
#11456=DIRECTION('ref_axis',(1.,0.,0.));
#11457=DIRECTION('center_axis',(0.,0.,1.));
#11458=DIRECTION('ref_axis',(1.,0.,0.));
#11459=DIRECTION('',(-1.,-1.22464679914735E-16,0.));
#11460=DIRECTION('',(-1.,-1.22464679914735E-16,0.));
#11461=DIRECTION('',(0.,1.,0.));
#11462=DIRECTION('center_axis',(0.,0.,-1.));
#11463=DIRECTION('ref_axis',(-1.,0.,0.));
#11464=DIRECTION('',(-1.,-6.64977332457776E-15,0.));
#11465=DIRECTION('center_axis',(0.,0.,-1.));
#11466=DIRECTION('ref_axis',(1.,0.,0.));
#11467=DIRECTION('',(0.,-1.,0.));
#11468=DIRECTION('center_axis',(0.,0.,-1.));
#11469=DIRECTION('ref_axis',(1.,0.,0.));
#11470=DIRECTION('center_axis',(0.,0.,-1.));
#11471=DIRECTION('ref_axis',(-1.,0.,0.));
#11472=DIRECTION('',(0.,-1.,0.));
#11473=DIRECTION('',(0.,-1.,0.));
#11474=DIRECTION('center_axis',(1.22464679914735E-16,-1.,0.));
#11475=DIRECTION('ref_axis',(1.,1.22464679914735E-16,0.));
#11476=DIRECTION('',(-1.,-1.22464679914735E-16,0.));
#11477=DIRECTION('',(0.,0.,-1.));
#11478=DIRECTION('',(0.,0.,-1.));
#11479=DIRECTION('center_axis',(-1.,0.,0.));
#11480=DIRECTION('ref_axis',(0.,0.,1.));
#11481=DIRECTION('',(0.,1.,0.));
#11482=DIRECTION('',(0.,0.,-1.));
#11483=DIRECTION('center_axis',(1.22464679914735E-16,-1.,0.));
#11484=DIRECTION('ref_axis',(1.,1.22464679914735E-16,0.));
#11485=DIRECTION('',(-1.,-1.22464679914735E-16,0.));
#11486=DIRECTION('',(0.,0.,-1.));
#11487=DIRECTION('center_axis',(0.,0.,-1.));
#11488=DIRECTION('ref_axis',(-1.,0.,0.));
#11489=DIRECTION('',(0.,0.,-1.));
#11490=DIRECTION('center_axis',(1.,0.,0.));
#11491=DIRECTION('ref_axis',(0.,0.,-1.));
#11492=DIRECTION('',(0.,0.,-1.));
#11493=DIRECTION('center_axis',(0.,0.,-1.));
#11494=DIRECTION('ref_axis',(-1.,0.,0.));
#11495=DIRECTION('',(0.,0.,-1.));
#11496=DIRECTION('center_axis',(0.457850135121644,0.889029388585716,0.));
#11497=DIRECTION('ref_axis',(-0.889029388585716,0.457850135121644,0.));
#11498=DIRECTION('',(0.,0.,-1.));
#11499=DIRECTION('center_axis',(0.,0.,-1.));
#11500=DIRECTION('ref_axis',(-1.,0.,0.));
#11501=DIRECTION('center_axis',(0.,0.,-1.));
#11502=DIRECTION('ref_axis',(-1.,0.,0.));
#11503=DIRECTION('',(0.,0.,-1.));
#11504=DIRECTION('center_axis',(-1.,0.,0.));
#11505=DIRECTION('ref_axis',(0.,0.,1.));
#11506=DIRECTION('',(0.,0.,-1.));
#11507=DIRECTION('center_axis',(0.,0.,-1.));
#11508=DIRECTION('ref_axis',(-1.,0.,0.));
#11509=DIRECTION('',(0.,0.,-1.));
#11510=DIRECTION('center_axis',(0.,-1.,0.));
#11511=DIRECTION('ref_axis',(0.,0.,-1.));
#11512=DIRECTION('',(0.,0.,-1.));
#11513=DIRECTION('',(-1.,0.,0.));
#11514=DIRECTION('center_axis',(1.,0.,0.));
#11515=DIRECTION('ref_axis',(0.,0.,-1.));
#11516=DIRECTION('',(0.,0.,-1.));
#11517=DIRECTION('',(0.,-1.,0.));
#11518=DIRECTION('center_axis',(0.,-1.,0.));
#11519=DIRECTION('ref_axis',(0.,0.,-1.));
#11520=DIRECTION('',(0.,0.,-1.));
#11521=DIRECTION('',(-1.,0.,0.));
#11522=DIRECTION('center_axis',(0.,0.,-1.));
#11523=DIRECTION('ref_axis',(-1.,0.,0.));
#11524=DIRECTION('',(0.,0.,-1.));
#11525=DIRECTION('center_axis',(-1.,0.,0.));
#11526=DIRECTION('ref_axis',(0.,0.,1.));
#11527=DIRECTION('',(0.,0.,-1.));
#11528=DIRECTION('center_axis',(0.,0.,-1.));
#11529=DIRECTION('ref_axis',(-1.,0.,0.));
#11530=DIRECTION('',(-8.67361737988404E-16,0.,-1.));
#11531=DIRECTION('',(0.,0.,-1.));
#11532=DIRECTION('center_axis',(0.,0.,-1.));
#11533=DIRECTION('ref_axis',(-1.,0.,0.));
#11534=DIRECTION('',(0.,0.,-1.));
#11535=DIRECTION('',(0.,0.,-1.));
#11536=DIRECTION('',(0.,0.,1.));
#11537=DIRECTION('center_axis',(0.457850135121644,0.889029388585716,0.));
#11538=DIRECTION('ref_axis',(-0.889029388585716,0.457850135121644,0.));
#11539=DIRECTION('',(0.,0.,-1.));
#11540=DIRECTION('center_axis',(0.,0.,-1.));
#11541=DIRECTION('ref_axis',(-1.,0.,0.));
#11542=DIRECTION('',(0.,0.,-1.));
#11543=DIRECTION('center_axis',(1.,0.,0.));
#11544=DIRECTION('ref_axis',(0.,0.,-1.));
#11545=DIRECTION('',(0.,0.,-1.));
#11546=DIRECTION('center_axis',(0.,0.,-1.));
#11547=DIRECTION('ref_axis',(-1.,0.,0.));
#11548=DIRECTION('center_axis',(0.,0.,1.));
#11549=DIRECTION('ref_axis',(1.,0.,0.));
#11550=DIRECTION('center_axis',(0.,0.,1.));
#11551=DIRECTION('ref_axis',(1.,0.,0.));
#11552=DIRECTION('center_axis',(1.,0.,0.));
#11553=DIRECTION('ref_axis',(0.,0.,-1.));
#11554=DIRECTION('center_axis',(1.,0.,0.));
#11555=DIRECTION('ref_axis',(0.,1.76941794549634E-13,1.));
#11556=DIRECTION('',(0.,0.,1.));
#11557=DIRECTION('center_axis',(1.,0.,0.));
#11558=DIRECTION('ref_axis',(0.,0.,1.));
#11559=DIRECTION('center_axis',(1.,0.,0.));
#11560=DIRECTION('ref_axis',(0.,0.,-1.));
#11561=DIRECTION('center_axis',(-1.,0.,0.));
#11562=DIRECTION('ref_axis',(0.,0.,1.));
#11563=DIRECTION('center_axis',(-1.,0.,0.));
#11564=DIRECTION('ref_axis',(0.,0.,1.));
#11565=DIRECTION('',(0.,0.,1.));
#11566=DIRECTION('center_axis',(-1.,0.,0.));
#11567=DIRECTION('ref_axis',(0.,3.46944695195361E-15,1.));
#11568=DIRECTION('',(1.,0.,0.));
#11569=DIRECTION('center_axis',(-1.,0.,0.));
#11570=DIRECTION('ref_axis',(0.,0.,1.));
#11571=DIRECTION('',(-1.,0.,0.));
#11572=DIRECTION('center_axis',(1.,0.,0.));
#11573=DIRECTION('ref_axis',(0.,0.,-1.));
#11574=DIRECTION('',(0.,-1.,3.89551938464967E-15));
#11575=DIRECTION('',(0.,-3.49148133884313E-15,-1.));
#11576=DIRECTION('',(0.,-1.,3.89551938464967E-15));
#11577=DIRECTION('center_axis',(-1.,0.,0.));
#11578=DIRECTION('ref_axis',(0.,0.,1.));
#11579=DIRECTION('',(0.,1.,-3.89551938464967E-15));
#11580=DIRECTION('',(0.,0.,1.));
#11581=DIRECTION('',(0.,1.,-3.89551938464967E-15));
#11582=DIRECTION('center_axis',(0.,-3.89551938464967E-15,-1.));
#11583=DIRECTION('ref_axis',(0.,1.,-3.89551938464967E-15));
#11584=DIRECTION('',(1.,0.,0.));
#11585=DIRECTION('',(0.,1.,0.));
#11586=DIRECTION('',(-0.889029388585716,0.457850135121644,0.));
#11587=DIRECTION('center_axis',(0.,-3.89551938464967E-15,-1.));
#11588=DIRECTION('ref_axis',(0.,1.,-3.89551938464967E-15));
#11589=DIRECTION('',(-0.889029388585716,0.457850135121644,0.));
#11590=DIRECTION('',(0.,1.,0.));
#11591=DIRECTION('',(1.,0.,0.));
#11592=DIRECTION('center_axis',(0.,1.,-3.49148133884313E-15));
#11593=DIRECTION('ref_axis',(0.,3.49148133884313E-15,1.));
#11594=DIRECTION('',(0.,0.,1.));
#11595=DIRECTION('center_axis',(0.457850135121644,0.889029388585716,0.));
#11596=DIRECTION('ref_axis',(-0.889029388585716,0.457850135121644,0.));
#11597=DIRECTION('',(0.,0.,1.));
#11598=DIRECTION('center_axis',(1.,0.,0.));
#11599=DIRECTION('ref_axis',(0.,0.,-1.));
#11600=DIRECTION('center_axis',(-1.,0.,0.));
#11601=DIRECTION('ref_axis',(0.,0.,1.));
#11602=DIRECTION('center_axis',(-1.,0.,0.));
#11603=DIRECTION('ref_axis',(0.,0.,-1.));
#11604=DIRECTION('center_axis',(-1.,0.,0.));
#11605=DIRECTION('ref_axis',(0.,0.,-1.));
#11606=DIRECTION('',(0.,6.98296267768627E-15,-1.));
#11607=DIRECTION('center_axis',(-1.,0.,0.));
#11608=DIRECTION('ref_axis',(0.,0.,1.));
#11609=DIRECTION('center_axis',(1.,0.,0.));
#11610=DIRECTION('ref_axis',(0.,0.,-1.));
#11611=DIRECTION('center_axis',(1.,0.,0.));
#11612=DIRECTION('ref_axis',(0.,0.,-1.));
#11613=DIRECTION('',(0.,6.98296267768627E-15,-1.));
#11614=DIRECTION('center_axis',(1.,0.,0.));
#11615=DIRECTION('ref_axis',(0.,3.46944695195361E-15,-1.));
#11616=DIRECTION('',(-1.,0.,0.));
#11617=DIRECTION('center_axis',(1.,0.,0.));
#11618=DIRECTION('ref_axis',(0.,0.,-1.));
#11619=DIRECTION('',(1.,0.,0.));
#11620=DIRECTION('center_axis',(1.,0.,0.));
#11621=DIRECTION('ref_axis',(0.,0.,-1.));
#11622=DIRECTION('',(0.,1.,3.49148133884313E-15));
#11623=DIRECTION('',(0.,-3.49148133884313E-15,1.));
#11624=DIRECTION('',(0.,1.,3.49148133884313E-15));
#11625=DIRECTION('center_axis',(-1.,0.,0.));
#11626=DIRECTION('ref_axis',(0.,0.,1.));
#11627=DIRECTION('',(0.,-1.,-3.49148133884313E-15));
#11628=DIRECTION('',(0.,3.49148133884313E-15,-1.));
#11629=DIRECTION('',(0.,-1.,-3.49148133884313E-15));
#11630=DIRECTION('center_axis',(0.,-3.49148133884313E-15,1.));
#11631=DIRECTION('ref_axis',(0.,-1.,-3.49148133884313E-15));
#11632=DIRECTION('',(0.889029388585716,-0.457850135121644,-1.59857520276403E-15));
#11633=DIRECTION('',(0.,-1.,-3.49148133884313E-15));
#11634=DIRECTION('',(-1.,0.,0.));
#11635=DIRECTION('center_axis',(0.,-3.49148133884313E-15,1.));
#11636=DIRECTION('ref_axis',(0.,-1.,-3.49148133884313E-15));
#11637=DIRECTION('',(-1.,0.,0.));
#11638=DIRECTION('',(0.,-1.,-3.49148133884313E-15));
#11639=DIRECTION('',(0.889029388585716,-0.457850135121644,-1.59857520276403E-15));
#11640=DIRECTION('center_axis',(0.,1.,3.49148133884313E-15));
#11641=DIRECTION('ref_axis',(0.,-3.49148133884313E-15,1.));
#11642=DIRECTION('',(0.,3.49148133884313E-15,-1.));
#11643=DIRECTION('center_axis',(1.,0.,0.));
#11644=DIRECTION('ref_axis',(0.,0.,-1.));
#11645=DIRECTION('',(0.,3.49148133884313E-15,-1.));
#11646=DIRECTION('center_axis',(0.457850135121644,0.889029388585716,3.10402951993015E-15));
#11647=DIRECTION('ref_axis',(-0.889029388585716,0.457850135121644,4.3777256771857E-32));
#11648=DIRECTION('axis',(0.,0.,1.));
#11649=DIRECTION('refdir',(1.,0.,0.));
#11650=DIRECTION('center_axis',(-1.,0.,0.));
#11651=DIRECTION('ref_axis',(0.,0.,1.));
#11652=DIRECTION('center_axis',(-1.,0.,0.));
#11653=DIRECTION('ref_axis',(0.,0.,1.));
#11654=DIRECTION('',(-1.,0.,0.));
#11655=DIRECTION('center_axis',(-1.,0.,0.));
#11656=DIRECTION('ref_axis',(0.,0.,1.));
#11657=DIRECTION('center_axis',(-1.,0.,0.));
#11658=DIRECTION('ref_axis',(0.,0.,1.));
#11659=DIRECTION('center_axis',(-1.,0.,0.));
#11660=DIRECTION('ref_axis',(0.,0.,1.));
#11661=DIRECTION('',(-1.,0.,0.));
#11662=DIRECTION('center_axis',(-1.,0.,0.));
#11663=DIRECTION('ref_axis',(0.,0.,1.));
#11664=DIRECTION('center_axis',(-1.,0.,0.));
#11665=DIRECTION('ref_axis',(0.,0.,1.));
#11666=DIRECTION('center_axis',(-1.,0.,0.));
#11667=DIRECTION('ref_axis',(0.,0.,1.));
#11668=DIRECTION('',(-1.,0.,0.));
#11669=DIRECTION('center_axis',(-1.,0.,0.));
#11670=DIRECTION('ref_axis',(0.,0.,1.));
#11671=DIRECTION('center_axis',(-1.,0.,0.));
#11672=DIRECTION('ref_axis',(0.,0.,1.));
#11673=DIRECTION('center_axis',(-1.,0.,0.));
#11674=DIRECTION('ref_axis',(0.,0.,1.));
#11675=DIRECTION('',(-1.,0.,0.));
#11676=DIRECTION('center_axis',(-1.,0.,0.));
#11677=DIRECTION('ref_axis',(0.,0.,1.));
#11678=DIRECTION('center_axis',(1.22464679914735E-16,-1.,0.));
#11679=DIRECTION('ref_axis',(1.,1.22464679914735E-16,0.));
#11680=DIRECTION('center_axis',(1.22464679914735E-16,-1.,0.));
#11681=DIRECTION('ref_axis',(1.,1.22464679914735E-16,0.));
#11682=DIRECTION('',(1.22464679914735E-16,-1.,0.));
#11683=DIRECTION('center_axis',(1.22464679914735E-16,-1.,0.));
#11684=DIRECTION('ref_axis',(1.,1.22464679914735E-16,0.));
#11685=DIRECTION('center_axis',(1.22464679914735E-16,-1.,0.));
#11686=DIRECTION('ref_axis',(1.,1.22464679914735E-16,0.));
#11687=DIRECTION('center_axis',(1.22464679914735E-16,-1.,0.));
#11688=DIRECTION('ref_axis',(1.,1.22464679914735E-16,0.));
#11689=DIRECTION('',(1.22464679914735E-16,-1.,0.));
#11690=DIRECTION('center_axis',(1.22464679914735E-16,-1.,0.));
#11691=DIRECTION('ref_axis',(-1.,-1.22464679914735E-16,0.));
#11692=DIRECTION('center_axis',(1.22464679914735E-16,-1.,0.));
#11693=DIRECTION('ref_axis',(1.,1.22464679914735E-16,0.));
#11694=DIRECTION('center_axis',(1.22464679914735E-16,-1.,0.));
#11695=DIRECTION('ref_axis',(1.,1.22464679914735E-16,0.));
#11696=DIRECTION('',(1.22464679914735E-16,-1.,0.));
#11697=DIRECTION('center_axis',(1.22464679914735E-16,-1.,0.));
#11698=DIRECTION('ref_axis',(1.,1.22464679914735E-16,0.));
#11699=DIRECTION('center_axis',(1.22464679914735E-16,-1.,0.));
#11700=DIRECTION('ref_axis',(1.,1.22464679914735E-16,0.));
#11701=DIRECTION('center_axis',(1.22464679914735E-16,-1.,0.));
#11702=DIRECTION('ref_axis',(1.,1.22464679914735E-16,0.));
#11703=DIRECTION('',(1.22464679914735E-16,-1.,0.));
#11704=DIRECTION('center_axis',(1.22464679914735E-16,-1.,0.));
#11705=DIRECTION('ref_axis',(1.,1.22464679914735E-16,0.));
#11706=DIRECTION('center_axis',(0.,0.,-1.));
#11707=DIRECTION('ref_axis',(-1.,0.,0.));
#11708=DIRECTION('',(1.,0.,0.));
#11709=DIRECTION('',(0.,-1.,0.));
#11710=DIRECTION('',(1.,0.,0.));
#11711=DIRECTION('',(0.,1.,0.));
#11712=DIRECTION('center_axis',(0.,0.,1.));
#11713=DIRECTION('ref_axis',(1.,0.,0.));
#11714=DIRECTION('',(0.,-1.,0.));
#11715=DIRECTION('center_axis',(0.,0.,-1.));
#11716=DIRECTION('ref_axis',(1.,0.,0.));
#11717=DIRECTION('',(1.,0.,0.));
#11718=DIRECTION('center_axis',(0.,0.,-1.));
#11719=DIRECTION('ref_axis',(1.,0.,0.));
#11720=DIRECTION('center_axis',(0.,0.,1.));
#11721=DIRECTION('ref_axis',(1.,0.,0.));
#11722=DIRECTION('',(-1.,-1.22464679914735E-16,0.));
#11723=DIRECTION('',(-1.,-1.22464679914735E-16,0.));
#11724=DIRECTION('',(1.22464679914735E-16,-1.,0.));
#11725=DIRECTION('center_axis',(0.,0.,-1.));
#11726=DIRECTION('ref_axis',(-1.,0.,0.));
#11727=DIRECTION('',(-1.,0.,0.));
#11728=DIRECTION('center_axis',(0.,0.,-1.));
#11729=DIRECTION('ref_axis',(1.,0.,0.));
#11730=DIRECTION('',(0.,1.,0.));
#11731=DIRECTION('center_axis',(0.,0.,-1.));
#11732=DIRECTION('ref_axis',(1.,0.,0.));
#11733=DIRECTION('center_axis',(0.,0.,-1.));
#11734=DIRECTION('ref_axis',(-1.,0.,0.));
#11735=DIRECTION('',(0.,1.,0.));
#11736=DIRECTION('',(0.,1.,0.));
#11737=DIRECTION('',(1.,0.,0.));
#11738=DIRECTION('center_axis',(0.,0.,1.));
#11739=DIRECTION('ref_axis',(1.,0.,0.));
#11740=DIRECTION('',(-1.,0.,0.));
#11741=DIRECTION('center_axis',(0.,0.,-1.));
#11742=DIRECTION('ref_axis',(1.,0.,0.));
#11743=DIRECTION('',(0.,-1.,0.));
#11744=DIRECTION('center_axis',(0.,0.,-1.));
#11745=DIRECTION('ref_axis',(1.,0.,0.));
#11746=DIRECTION('center_axis',(0.,0.,1.));
#11747=DIRECTION('ref_axis',(1.,0.,0.));
#11748=DIRECTION('',(0.,1.,0.));
#11749=DIRECTION('',(0.,1.,0.));
#11750=DIRECTION('center_axis',(0.,0.,-1.));
#11751=DIRECTION('ref_axis',(-1.,0.,0.));
#11752=DIRECTION('center_axis',(0.,0.,-1.));
#11753=DIRECTION('ref_axis',(1.,0.,0.));
#11754=DIRECTION('center_axis',(0.,0.,-1.));
#11755=DIRECTION('ref_axis',(1.,0.,0.));
#11756=DIRECTION('center_axis',(0.,0.,1.));
#11757=DIRECTION('ref_axis',(1.,0.,0.));
#11758=DIRECTION('',(0.,-1.,0.));
#11759=DIRECTION('',(1.,0.,0.));
#11760=DIRECTION('',(1.,0.,0.));
#11761=DIRECTION('center_axis',(1.,-3.65204942310907E-16,0.));
#11762=DIRECTION('ref_axis',(3.65204942310907E-16,1.,0.));
#11763=DIRECTION('',(0.,0.,-1.));
#11764=DIRECTION('',(-1.68975972140531E-16,-0.462688076101332,0.886521147087675));
#11765=DIRECTION('',(0.,0.,-1.));
#11766=DIRECTION('',(1.71139076064604E-16,0.468611062549393,0.883404591371547));
#11767=DIRECTION('center_axis',(0.,-1.,0.));
#11768=DIRECTION('ref_axis',(0.,0.,-1.));
#11769=DIRECTION('',(1.,0.,0.));
#11770=DIRECTION('',(0.,0.,-1.));
#11771=DIRECTION('',(1.,0.,0.));
#11772=DIRECTION('center_axis',(1.,-3.65204942310907E-16,0.));
#11773=DIRECTION('ref_axis',(3.65204942310907E-16,1.,0.));
#11774=DIRECTION('',(0.,-0.462688076101332,0.886521147087675));
#11775=DIRECTION('',(0.,0.,-1.));
#11776=DIRECTION('',(0.,0.468611062549393,0.883404591371547));
#11777=DIRECTION('center_axis',(0.,0.,-1.));
#11778=DIRECTION('ref_axis',(0.707106781186548,0.707106781186547,0.));
#11779=DIRECTION('center_axis',(-9.04452389970748E-15,-0.886521147087677,
-0.462688076101329));
#11780=DIRECTION('ref_axis',(8.69090002824443E-14,0.462688076101329,-0.886521147087677));
#11781=DIRECTION('',(0.,0.,-1.));
#11782=DIRECTION('center_axis',(-1.79450933059916E-14,-0.88340459137155,
0.468611062549386));
#11783=DIRECTION('ref_axis',(1.21092278199327E-14,-0.468611062549386,-0.88340459137155));
#11784=DIRECTION('center_axis',(0.,1.,0.));
#11785=DIRECTION('ref_axis',(0.,0.,1.));
#11786=DIRECTION('',(1.,0.,0.));
#11787=DIRECTION('',(0.,0.,-1.));
#11788=DIRECTION('',(0.,0.,-1.));
#11789=DIRECTION('',(0.,0.,1.));
#11790=DIRECTION('',(-1.,0.,0.));
#11791=DIRECTION('center_axis',(0.,0.,-1.));
#11792=DIRECTION('ref_axis',(-1.,0.,0.));
#11793=DIRECTION('',(0.,0.,-1.));
#11794=DIRECTION('center_axis',(-1.,0.,0.));
#11795=DIRECTION('ref_axis',(0.,0.,1.));
#11796=DIRECTION('',(0.,0.,-1.));
#11797=DIRECTION('center_axis',(0.,0.,-1.));
#11798=DIRECTION('ref_axis',(-1.,0.,0.));
#11799=DIRECTION('',(0.,0.,-1.));
#11800=DIRECTION('center_axis',(1.22464679914735E-16,-1.,0.));
#11801=DIRECTION('ref_axis',(1.,1.22464679914735E-16,0.));
#11802=DIRECTION('',(-1.,-1.22464679914735E-16,0.));
#11803=DIRECTION('',(0.,0.,-1.));
#11804=DIRECTION('center_axis',(1.,1.22464679914735E-16,0.));
#11805=DIRECTION('ref_axis',(-1.22464679914735E-16,1.,0.));
#11806=DIRECTION('',(1.22464679914735E-16,-1.,0.));
#11807=DIRECTION('',(0.,0.,-1.));
#11808=DIRECTION('center_axis',(1.22464679914735E-16,-1.,0.));
#11809=DIRECTION('ref_axis',(1.,1.22464679914735E-16,0.));
#11810=DIRECTION('',(-1.,-1.22464679914735E-16,0.));
#11811=DIRECTION('',(0.,0.,-1.));
#11812=DIRECTION('center_axis',(0.,0.,-1.));
#11813=DIRECTION('ref_axis',(-1.,0.,0.));
#11814=DIRECTION('',(0.,0.,-1.));
#11815=DIRECTION('center_axis',(-1.,0.,0.));
#11816=DIRECTION('ref_axis',(0.,0.,1.));
#11817=DIRECTION('',(0.,0.,-1.));
#11818=DIRECTION('center_axis',(0.,0.,-1.));
#11819=DIRECTION('ref_axis',(-1.,0.,0.));
#11820=DIRECTION('',(0.,0.,-1.));
#11821=DIRECTION('center_axis',(0.,1.,0.));
#11822=DIRECTION('ref_axis',(0.,0.,1.));
#11823=DIRECTION('',(0.,0.,-1.));
#11824=DIRECTION('',(1.,0.,0.));
#11825=DIRECTION('',(0.,0.,-1.));
#11826=DIRECTION('',(-1.,0.,0.));
#11827=DIRECTION('',(0.,0.,1.));
#11828=DIRECTION('center_axis',(0.,0.,-1.));
#11829=DIRECTION('ref_axis',(-1.,0.,0.));
#11830=DIRECTION('center_axis',(-2.77796091205298E-14,-0.886521147087676,
-0.462688076101331));
#11831=DIRECTION('ref_axis',(6.62185632336808E-14,0.462688076101331,-0.886521147087676));
#11832=DIRECTION('center_axis',(1.88700981155792E-14,-0.883404591371546,
0.468611062549393));
#11833=DIRECTION('ref_axis',(3.43055792298147E-13,-0.468611062549393,-0.883404591371546));
#11834=DIRECTION('center_axis',(0.,0.,1.));
#11835=DIRECTION('ref_axis',(1.,0.,0.));
#11836=DIRECTION('center_axis',(-1.,0.,0.));
#11837=DIRECTION('ref_axis',(0.,0.,1.));
#11838=DIRECTION('',(0.,0.468611062549393,0.883404591371547));
#11839=DIRECTION('center_axis',(0.,0.883404591371547,-0.468611062549393));
#11840=DIRECTION('ref_axis',(0.,0.468611062549393,0.883404591371547));
#11841=DIRECTION('center_axis',(0.,0.886521147087676,0.462688076101332));
#11842=DIRECTION('ref_axis',(0.,-0.462688076101332,0.886521147087676));
#11843=DIRECTION('',(0.,-0.462688076101332,0.886521147087675));
#11844=DIRECTION('center_axis',(1.,0.,0.));
#11845=DIRECTION('ref_axis',(0.,0.,-1.));
#11846=DIRECTION('axis',(0.,0.,1.));
#11847=DIRECTION('refdir',(1.,0.,0.));
#11848=DIRECTION('center_axis',(-1.,0.,0.));
#11849=DIRECTION('ref_axis',(0.,0.,1.));
#11850=DIRECTION('center_axis',(-1.,0.,0.));
#11851=DIRECTION('ref_axis',(0.,0.,1.));
#11852=DIRECTION('',(-1.,0.,0.));
#11853=DIRECTION('center_axis',(-1.,0.,0.));
#11854=DIRECTION('ref_axis',(0.,0.,1.));
#11855=DIRECTION('center_axis',(-1.,0.,0.));
#11856=DIRECTION('ref_axis',(0.,0.,-1.));
#11857=DIRECTION('center_axis',(1.,0.,0.));
#11858=DIRECTION('ref_axis',(0.,0.,-1.));
#11859=DIRECTION('',(-1.,0.,0.));
#11860=DIRECTION('center_axis',(1.,0.,0.));
#11861=DIRECTION('ref_axis',(0.,0.,-1.));
#11862=DIRECTION('center_axis',(-1.,0.,0.));
#11863=DIRECTION('ref_axis',(0.,0.,-1.));
#11864=DIRECTION('center_axis',(1.,0.,0.));
#11865=DIRECTION('ref_axis',(0.,0.,-1.));
#11866=DIRECTION('',(-1.,0.,0.));
#11867=DIRECTION('center_axis',(1.,0.,0.));
#11868=DIRECTION('ref_axis',(0.,0.,-1.));
#11869=DIRECTION('center_axis',(-1.,0.,0.));
#11870=DIRECTION('ref_axis',(0.,0.,-1.));
#11871=DIRECTION('center_axis',(1.,0.,0.));
#11872=DIRECTION('ref_axis',(0.,0.,-1.));
#11873=DIRECTION('',(-1.,0.,0.));
#11874=DIRECTION('center_axis',(1.,0.,0.));
#11875=DIRECTION('ref_axis',(0.,0.,-1.));
#11876=DIRECTION('center_axis',(1.22464679914735E-16,-1.,0.));
#11877=DIRECTION('ref_axis',(1.,1.22464679914735E-16,0.));
#11878=DIRECTION('center_axis',(-1.22464679914735E-16,1.,0.));
#11879=DIRECTION('ref_axis',(1.,1.22464679914735E-16,0.));
#11880=DIRECTION('',(1.22464679914735E-16,-1.,0.));
#11881=DIRECTION('center_axis',(-1.22464679914735E-16,1.,0.));
#11882=DIRECTION('ref_axis',(1.,1.22464679914735E-16,0.));
#11883=DIRECTION('center_axis',(1.22464679914735E-16,-1.,0.));
#11884=DIRECTION('ref_axis',(1.,1.22464679914735E-16,0.));
#11885=DIRECTION('center_axis',(-1.22464679914735E-16,1.,0.));
#11886=DIRECTION('ref_axis',(1.,1.22464679914735E-16,0.));
#11887=DIRECTION('',(1.22464679914735E-16,-1.,0.));
#11888=DIRECTION('center_axis',(-1.22464679914735E-16,1.,0.));
#11889=DIRECTION('ref_axis',(-1.,-1.22464679914735E-16,0.));
#11890=DIRECTION('center_axis',(1.22464679914735E-16,-1.,0.));
#11891=DIRECTION('ref_axis',(1.,1.22464679914735E-16,0.));
#11892=DIRECTION('center_axis',(-1.22464679914735E-16,1.,0.));
#11893=DIRECTION('ref_axis',(1.,1.22464679914735E-16,0.));
#11894=DIRECTION('',(1.22464679914735E-16,-1.,0.));
#11895=DIRECTION('center_axis',(-1.22464679914735E-16,1.,0.));
#11896=DIRECTION('ref_axis',(1.,1.22464679914735E-16,0.));
#11897=DIRECTION('center_axis',(1.22464679914735E-16,-1.,0.));
#11898=DIRECTION('ref_axis',(1.,1.22464679914735E-16,0.));
#11899=DIRECTION('center_axis',(-1.22464679914735E-16,1.,0.));
#11900=DIRECTION('ref_axis',(1.,1.22464679914735E-16,0.));
#11901=DIRECTION('',(1.22464679914735E-16,-1.,0.));
#11902=DIRECTION('center_axis',(-1.22464679914735E-16,1.,0.));
#11903=DIRECTION('ref_axis',(1.,1.22464679914735E-16,0.));
#11904=DIRECTION('center_axis',(0.,0.,1.));
#11905=DIRECTION('ref_axis',(-1.,0.,0.));
#11906=DIRECTION('',(1.,0.,0.));
#11907=DIRECTION('',(0.,1.,0.));
#11908=DIRECTION('',(1.,0.,0.));
#11909=DIRECTION('',(0.,-1.,0.));
#11910=DIRECTION('center_axis',(0.,0.,-1.));
#11911=DIRECTION('ref_axis',(1.,0.,0.));
#11912=DIRECTION('',(0.,-1.,0.));
#11913=DIRECTION('center_axis',(0.,0.,-1.));
#11914=DIRECTION('ref_axis',(1.,0.,0.));
#11915=DIRECTION('',(1.,0.,0.));
#11916=DIRECTION('center_axis',(0.,0.,-1.));
#11917=DIRECTION('ref_axis',(1.,0.,0.));
#11918=DIRECTION('center_axis',(0.,0.,-1.));
#11919=DIRECTION('ref_axis',(1.,0.,0.));
#11920=DIRECTION('',(-1.,-1.22464679914735E-16,0.));
#11921=DIRECTION('',(1.22464679914735E-16,-1.,0.));
#11922=DIRECTION('',(-1.,-1.22464679914735E-16,0.));
#11923=DIRECTION('center_axis',(0.,0.,1.));
#11924=DIRECTION('ref_axis',(-1.,0.,0.));
#11925=DIRECTION('',(-1.,0.,0.));
#11926=DIRECTION('center_axis',(0.,0.,-1.));
#11927=DIRECTION('ref_axis',(1.,0.,0.));
#11928=DIRECTION('',(0.,1.,0.));
#11929=DIRECTION('center_axis',(0.,0.,-1.));
#11930=DIRECTION('ref_axis',(1.,0.,0.));
#11931=DIRECTION('center_axis',(0.,0.,1.));
#11932=DIRECTION('ref_axis',(-1.,0.,0.));
#11933=DIRECTION('',(0.,1.,0.));
#11934=DIRECTION('',(1.,0.,0.));
#11935=DIRECTION('',(0.,1.,0.));
#11936=DIRECTION('center_axis',(0.,0.,-1.));
#11937=DIRECTION('ref_axis',(1.,0.,0.));
#11938=DIRECTION('',(-1.,0.,0.));
#11939=DIRECTION('center_axis',(0.,0.,-1.));
#11940=DIRECTION('ref_axis',(1.,0.,0.));
#11941=DIRECTION('',(0.,-1.,0.));
#11942=DIRECTION('center_axis',(0.,0.,-1.));
#11943=DIRECTION('ref_axis',(1.,0.,0.));
#11944=DIRECTION('center_axis',(0.,0.,-1.));
#11945=DIRECTION('ref_axis',(1.,0.,0.));
#11946=DIRECTION('',(0.,1.,0.));
#11947=DIRECTION('',(0.,1.,0.));
#11948=DIRECTION('center_axis',(0.,0.,1.));
#11949=DIRECTION('ref_axis',(-1.,0.,0.));
#11950=DIRECTION('center_axis',(0.,0.,-1.));
#11951=DIRECTION('ref_axis',(1.,0.,0.));
#11952=DIRECTION('center_axis',(0.,0.,-1.));
#11953=DIRECTION('ref_axis',(1.,0.,0.));
#11954=DIRECTION('center_axis',(0.,0.,-1.));
#11955=DIRECTION('ref_axis',(1.,0.,0.));
#11956=DIRECTION('',(0.,-1.,0.));
#11957=DIRECTION('',(1.,0.,0.));
#11958=DIRECTION('',(1.,0.,0.));
#11959=DIRECTION('center_axis',(1.,-3.65204942310907E-16,0.));
#11960=DIRECTION('ref_axis',(3.65204942310907E-16,1.,0.));
#11961=DIRECTION('',(0.,0.,1.));
#11962=DIRECTION('',(1.71139076064604E-16,0.468611062549393,-0.883404591371547));
#11963=DIRECTION('',(0.,0.,1.));
#11964=DIRECTION('',(-1.68975972140531E-16,-0.462688076101332,-0.886521147087675));
#11965=DIRECTION('center_axis',(0.,-1.,0.));
#11966=DIRECTION('ref_axis',(0.,0.,1.));
#11967=DIRECTION('',(1.,0.,0.));
#11968=DIRECTION('',(1.,0.,0.));
#11969=DIRECTION('',(0.,0.,1.));
#11970=DIRECTION('center_axis',(1.,-3.65204942310907E-16,0.));
#11971=DIRECTION('ref_axis',(3.65204942310907E-16,1.,0.));
#11972=DIRECTION('',(0.,-0.462688076101332,-0.886521147087675));
#11973=DIRECTION('',(0.,0.468611062549393,-0.883404591371547));
#11974=DIRECTION('',(0.,0.,1.));
#11975=DIRECTION('center_axis',(0.,0.,1.));
#11976=DIRECTION('ref_axis',(-1.,0.,0.));
#11977=DIRECTION('center_axis',(9.04452389970748E-15,0.886521147087677,
-0.462688076101329));
#11978=DIRECTION('ref_axis',(8.69090002824443E-14,0.462688076101329,0.886521147087677));
#11979=DIRECTION('center_axis',(1.79450933059916E-14,0.88340459137155,0.468611062549386));
#11980=DIRECTION('ref_axis',(1.21092278199327E-14,-0.468611062549386,0.88340459137155));
#11981=DIRECTION('',(0.,0.,1.));
#11982=DIRECTION('center_axis',(0.,1.,0.));
#11983=DIRECTION('ref_axis',(0.,0.,-1.));
#11984=DIRECTION('',(1.,0.,0.));
#11985=DIRECTION('',(-1.,0.,0.));
#11986=DIRECTION('',(0.,0.,-1.));
#11987=DIRECTION('',(0.,0.,1.));
#11988=DIRECTION('',(0.,0.,1.));
#11989=DIRECTION('center_axis',(0.,0.,1.));
#11990=DIRECTION('ref_axis',(-1.,0.,0.));
#11991=DIRECTION('',(0.,0.,1.));
#11992=DIRECTION('center_axis',(-1.,0.,0.));
#11993=DIRECTION('ref_axis',(0.,0.,-1.));
#11994=DIRECTION('',(0.,0.,1.));
#11995=DIRECTION('center_axis',(0.,0.,1.));
#11996=DIRECTION('ref_axis',(-1.,0.,0.));
#11997=DIRECTION('',(0.,0.,1.));
#11998=DIRECTION('center_axis',(1.22464679914735E-16,-1.,0.));
#11999=DIRECTION('ref_axis',(1.,1.22464679914735E-16,0.));
#12000=DIRECTION('',(-1.,-1.22464679914735E-16,0.));
#12001=DIRECTION('',(0.,0.,1.));
#12002=DIRECTION('center_axis',(1.,1.22464679914735E-16,0.));
#12003=DIRECTION('ref_axis',(-1.22464679914735E-16,1.,0.));
#12004=DIRECTION('',(1.22464679914735E-16,-1.,0.));
#12005=DIRECTION('',(0.,0.,1.));
#12006=DIRECTION('center_axis',(1.22464679914735E-16,-1.,0.));
#12007=DIRECTION('ref_axis',(1.,1.22464679914735E-16,0.));
#12008=DIRECTION('',(-1.,-1.22464679914735E-16,0.));
#12009=DIRECTION('',(0.,0.,1.));
#12010=DIRECTION('center_axis',(0.,0.,1.));
#12011=DIRECTION('ref_axis',(-1.,0.,0.));
#12012=DIRECTION('',(0.,0.,1.));
#12013=DIRECTION('center_axis',(-1.,0.,0.));
#12014=DIRECTION('ref_axis',(0.,0.,-1.));
#12015=DIRECTION('',(0.,0.,1.));
#12016=DIRECTION('center_axis',(0.,0.,1.));
#12017=DIRECTION('ref_axis',(-1.,0.,0.));
#12018=DIRECTION('',(0.,0.,1.));
#12019=DIRECTION('center_axis',(0.,1.,0.));
#12020=DIRECTION('ref_axis',(0.,0.,-1.));
#12021=DIRECTION('',(0.,0.,1.));
#12022=DIRECTION('',(0.,0.,-1.));
#12023=DIRECTION('',(-1.,0.,0.));
#12024=DIRECTION('',(0.,0.,1.));
#12025=DIRECTION('',(1.,0.,0.));
#12026=DIRECTION('center_axis',(0.,0.,1.));
#12027=DIRECTION('ref_axis',(-1.,0.,0.));
#12028=DIRECTION('center_axis',(-1.88700981155792E-14,0.883404591371546,
0.468611062549393));
#12029=DIRECTION('ref_axis',(3.43055792298147E-13,-0.468611062549393,0.883404591371546));
#12030=DIRECTION('center_axis',(2.77796091205298E-14,0.886521147087676,
-0.462688076101331));
#12031=DIRECTION('ref_axis',(6.62185632336808E-14,0.462688076101331,0.886521147087676));
#12032=DIRECTION('center_axis',(0.,0.,-1.));
#12033=DIRECTION('ref_axis',(1.,0.,0.));
#12034=DIRECTION('center_axis',(-1.,0.,0.));
#12035=DIRECTION('ref_axis',(0.,0.,-1.));
#12036=DIRECTION('',(0.,0.468611062549393,-0.883404591371547));
#12037=DIRECTION('center_axis',(0.,0.883404591371547,0.468611062549393));
#12038=DIRECTION('ref_axis',(0.,0.468611062549393,-0.883404591371547));
#12039=DIRECTION('center_axis',(0.,0.886521147087676,-0.462688076101332));
#12040=DIRECTION('ref_axis',(0.,-0.462688076101332,-0.886521147087676));
#12041=DIRECTION('',(0.,-0.462688076101332,-0.886521147087675));
#12042=DIRECTION('center_axis',(1.,0.,0.));
#12043=DIRECTION('ref_axis',(0.,0.,1.));
#12044=DIRECTION('axis',(0.,0.,1.));
#12045=DIRECTION('refdir',(1.,0.,0.));
#12046=DIRECTION('center_axis',(0.,1.,0.));
#12047=DIRECTION('ref_axis',(0.,0.,1.));
#12048=DIRECTION('center_axis',(0.,1.,0.));
#12049=DIRECTION('ref_axis',(0.,0.,1.));
#12050=DIRECTION('',(0.,1.,0.));
#12051=DIRECTION('center_axis',(0.,1.,0.));
#12052=DIRECTION('ref_axis',(0.,0.,1.));
#12053=DIRECTION('center_axis',(0.,1.,0.));
#12054=DIRECTION('ref_axis',(0.,0.,1.));
#12055=DIRECTION('center_axis',(0.,1.,0.));
#12056=DIRECTION('ref_axis',(0.,0.,1.));
#12057=DIRECTION('',(0.,1.,0.));
#12058=DIRECTION('center_axis',(0.,1.,0.));
#12059=DIRECTION('ref_axis',(0.,0.,-1.));
#12060=DIRECTION('center_axis',(0.,1.,0.));
#12061=DIRECTION('ref_axis',(0.,0.,1.));
#12062=DIRECTION('center_axis',(0.,1.,0.));
#12063=DIRECTION('ref_axis',(0.,0.,1.));
#12064=DIRECTION('',(0.,1.,0.));
#12065=DIRECTION('center_axis',(0.,1.,0.));
#12066=DIRECTION('ref_axis',(0.,0.,1.));
#12067=DIRECTION('center_axis',(0.,0.,1.));
#12068=DIRECTION('ref_axis',(1.,0.,0.));
#12069=DIRECTION('',(1.,-9.10615997888087E-17,0.));
#12070=DIRECTION('center_axis',(0.,0.,1.));
#12071=DIRECTION('ref_axis',(-1.,0.,0.));
#12072=DIRECTION('',(0.,1.,0.));
#12073=DIRECTION('center_axis',(0.,0.,1.));
#12074=DIRECTION('ref_axis',(1.,0.,0.));
#12075=DIRECTION('center_axis',(0.,0.,1.));
#12076=DIRECTION('ref_axis',(1.,0.,0.));
#12077=DIRECTION('',(0.,1.,0.));
#12078=DIRECTION('',(0.,1.,0.));
#12079=DIRECTION('',(-1.,0.,0.));
#12080=DIRECTION('center_axis',(0.,0.,-1.));
#12081=DIRECTION('ref_axis',(-1.,0.,0.));
#12082=DIRECTION('',(0.,-1.,0.));
#12083=DIRECTION('center_axis',(0.,0.,1.));
#12084=DIRECTION('ref_axis',(-1.,0.,0.));
#12085=DIRECTION('',(-1.,9.10615997888087E-17,0.));
#12086=DIRECTION('center_axis',(0.,0.,1.));
#12087=DIRECTION('ref_axis',(1.,0.,0.));
#12088=DIRECTION('center_axis',(0.,0.,-1.));
#12089=DIRECTION('ref_axis',(-1.,0.,0.));
#12090=DIRECTION('',(1.,0.,0.));
#12091=DIRECTION('',(1.,0.,0.));
#12092=DIRECTION('',(0.,1.,0.));
#12093=DIRECTION('center_axis',(0.,0.,1.));
#12094=DIRECTION('ref_axis',(1.,0.,0.));
#12095=DIRECTION('',(0.,-1.,0.));
#12096=DIRECTION('center_axis',(0.,0.,-1.));
#12097=DIRECTION('ref_axis',(1.,0.,0.));
#12098=DIRECTION('center_axis',(0.,0.,-1.));
#12099=DIRECTION('ref_axis',(1.,0.,0.));
#12100=DIRECTION('center_axis',(0.,0.,1.));
#12101=DIRECTION('ref_axis',(1.,0.,0.));
#12102=DIRECTION('',(1.,0.,0.));
#12103=DIRECTION('',(1.,0.,0.));
#12104=DIRECTION('',(0.,1.,0.));
#12105=DIRECTION('center_axis',(0.,0.,-1.));
#12106=DIRECTION('ref_axis',(-1.,0.,0.));
#12107=DIRECTION('',(1.,0.,0.));
#12108=DIRECTION('center_axis',(0.,0.,-1.));
#12109=DIRECTION('ref_axis',(1.,0.,0.));
#12110=DIRECTION('',(0.,1.,0.));
#12111=DIRECTION('center_axis',(0.,0.,-1.));
#12112=DIRECTION('ref_axis',(1.,0.,0.));
#12113=DIRECTION('center_axis',(0.,0.,-1.));
#12114=DIRECTION('ref_axis',(-1.,0.,0.));
#12115=DIRECTION('',(0.,1.,0.));
#12116=DIRECTION('',(0.,1.,0.));
#12117=DIRECTION('center_axis',(0.,0.,1.));
#12118=DIRECTION('ref_axis',(1.,0.,0.));
#12119=DIRECTION('',(-1.,0.,0.));
#12120=DIRECTION('center_axis',(0.,0.,-1.));
#12121=DIRECTION('ref_axis',(1.,0.,0.));
#12122=DIRECTION('center_axis',(0.,0.,-1.));
#12123=DIRECTION('ref_axis',(1.,0.,0.));
#12124=DIRECTION('center_axis',(0.,0.,1.));
#12125=DIRECTION('ref_axis',(1.,0.,0.));
#12126=DIRECTION('',(-1.,0.,0.));
#12127=DIRECTION('',(0.,-1.,0.));
#12128=DIRECTION('',(0.,-1.,0.));
#12129=DIRECTION('center_axis',(0.,0.,-1.));
#12130=DIRECTION('ref_axis',(-1.,0.,0.));
#12131=DIRECTION('',(0.,-1.,0.));
#12132=DIRECTION('center_axis',(0.,0.,-1.));
#12133=DIRECTION('ref_axis',(1.,0.,0.));
#12134=DIRECTION('',(1.,0.,0.));
#12135=DIRECTION('center_axis',(0.,0.,-1.));
#12136=DIRECTION('ref_axis',(1.,0.,0.));
#12137=DIRECTION('center_axis',(0.,0.,-1.));
#12138=DIRECTION('ref_axis',(-1.,0.,0.));
#12139=DIRECTION('',(1.,0.,0.));
#12140=DIRECTION('',(1.,0.,0.));
#12141=DIRECTION('center_axis',(0.,0.,-1.));
#12142=DIRECTION('ref_axis',(-1.,0.,0.));
#12143=DIRECTION('',(-1.,0.,0.));
#12144=DIRECTION('',(0.,-1.,0.));
#12145=DIRECTION('',(0.,-1.,0.));
#12146=DIRECTION('center_axis',(0.,1.,0.));
#12147=DIRECTION('ref_axis',(0.,0.,1.));
#12148=DIRECTION('',(0.,0.,-1.));
#12149=DIRECTION('',(-1.,0.,0.));
#12150=DIRECTION('',(0.,0.,-1.));
#12151=DIRECTION('',(-1.,0.,0.));
#12152=DIRECTION('center_axis',(1.,0.,0.));
#12153=DIRECTION('ref_axis',(0.,0.,-1.));
#12154=DIRECTION('',(0.,1.,0.));
#12155=DIRECTION('',(0.,-1.,0.));
#12156=DIRECTION('',(0.,0.,-1.));
#12157=DIRECTION('center_axis',(0.,1.,0.));
#12158=DIRECTION('ref_axis',(0.,0.,1.));
#12159=DIRECTION('',(-1.,0.,0.));
#12160=DIRECTION('',(1.,0.,0.));
#12161=DIRECTION('',(0.,0.,-1.));
#12162=DIRECTION('center_axis',(0.,0.,-1.));
#12163=DIRECTION('ref_axis',(-1.,0.,0.));
#12164=DIRECTION('center_axis',(0.,0.,-1.));
#12165=DIRECTION('ref_axis',(-1.,0.,0.));
#12166=DIRECTION('center_axis',(0.,0.,1.));
#12167=DIRECTION('ref_axis',(1.,0.,0.));
#12168=DIRECTION('',(0.,0.,-1.));
#12169=DIRECTION('center_axis',(1.,0.,0.));
#12170=DIRECTION('ref_axis',(0.,0.,-1.));
#12171=DIRECTION('',(0.,1.,0.));
#12172=DIRECTION('',(0.,-1.,0.));
#12173=DIRECTION('',(0.,0.,1.));
#12174=DIRECTION('',(0.,0.,-1.));
#12175=DIRECTION('',(0.,0.,1.));
#12176=DIRECTION('center_axis',(0.,0.,-1.));
#12177=DIRECTION('ref_axis',(-1.,0.,0.));
#12178=DIRECTION('',(0.,0.,-1.));
#12179=DIRECTION('center_axis',(0.,1.,0.));
#12180=DIRECTION('ref_axis',(0.,0.,1.));
#12181=DIRECTION('',(0.,0.,-1.));
#12182=DIRECTION('center_axis',(0.,0.,-1.));
#12183=DIRECTION('ref_axis',(-1.,0.,0.));
#12184=DIRECTION('',(0.,0.,-1.));
#12185=DIRECTION('center_axis',(-1.,0.,0.));
#12186=DIRECTION('ref_axis',(0.,0.,1.));
#12187=DIRECTION('',(0.,0.,-1.));
#12188=DIRECTION('center_axis',(0.,0.,-1.));
#12189=DIRECTION('ref_axis',(-1.,0.,0.));
#12190=DIRECTION('',(0.,0.,-1.));
#12191=DIRECTION('center_axis',(0.,1.,0.));
#12192=DIRECTION('ref_axis',(0.,0.,1.));
#12193=DIRECTION('',(0.,0.,-1.));
#12194=DIRECTION('',(1.,0.,0.));
#12195=DIRECTION('center_axis',(-1.,0.,0.));
#12196=DIRECTION('ref_axis',(0.,0.,1.));
#12197=DIRECTION('',(0.,0.,-1.));
#12198=DIRECTION('',(0.,1.,0.));
#12199=DIRECTION('center_axis',(0.,1.,0.));
#12200=DIRECTION('ref_axis',(0.,0.,1.));
#12201=DIRECTION('',(0.,0.,-1.));
#12202=DIRECTION('',(1.,0.,0.));
#12203=DIRECTION('center_axis',(0.,0.,-1.));
#12204=DIRECTION('ref_axis',(-1.,0.,0.));
#12205=DIRECTION('',(0.,0.,-1.));
#12206=DIRECTION('center_axis',(-1.,0.,0.));
#12207=DIRECTION('ref_axis',(0.,0.,1.));
#12208=DIRECTION('',(0.,0.,-1.));
#12209=DIRECTION('center_axis',(0.,0.,-1.));
#12210=DIRECTION('ref_axis',(-1.,0.,0.));
#12211=DIRECTION('',(0.,0.,-1.));
#12212=DIRECTION('center_axis',(0.,1.,0.));
#12213=DIRECTION('ref_axis',(0.,0.,1.));
#12214=DIRECTION('',(0.,0.,-1.));
#12215=DIRECTION('center_axis',(0.,0.,-1.));
#12216=DIRECTION('ref_axis',(-1.,0.,0.));
#12217=DIRECTION('',(0.,0.,-1.));
#12218=DIRECTION('center_axis',(1.,0.,0.));
#12219=DIRECTION('ref_axis',(0.,0.,-1.));
#12220=DIRECTION('',(0.,0.,-1.));
#12221=DIRECTION('',(0.,-1.,0.));
#12222=DIRECTION('',(0.,0.,-1.));
#12223=DIRECTION('',(0.,0.,-1.));
#12224=DIRECTION('',(0.,1.,0.));
#12225=DIRECTION('center_axis',(0.,0.,-1.));
#12226=DIRECTION('ref_axis',(-1.,0.,0.));
#12227=DIRECTION('center_axis',(0.,0.,-1.));
#12228=DIRECTION('ref_axis',(-1.,0.,0.));
#12229=DIRECTION('center_axis',(0.,0.,1.));
#12230=DIRECTION('ref_axis',(1.,0.,0.));
#12231=DIRECTION('center_axis',(0.,0.,-1.));
#12232=DIRECTION('ref_axis',(-1.,0.,0.));
#12233=DIRECTION('center_axis',(0.,0.,1.));
#12234=DIRECTION('ref_axis',(1.,0.,0.));
#12235=DIRECTION('',(-1.,0.,0.));
#12236=DIRECTION('center_axis',(0.,1.,0.));
#12237=DIRECTION('ref_axis',(0.,0.,1.));
#12238=DIRECTION('center_axis',(0.,0.,-1.));
#12239=DIRECTION('ref_axis',(-1.,0.,0.));
#12240=DIRECTION('',(-1.,0.,0.));
#12241=DIRECTION('center_axis',(0.,1.,0.));
#12242=DIRECTION('ref_axis',(0.,0.,1.));
#12243=DIRECTION('axis',(0.,0.,1.));
#12244=DIRECTION('refdir',(1.,0.,0.));
#12245=DIRECTION('center_axis',(0.,0.,1.));
#12246=DIRECTION('ref_axis',(1.,0.,0.));
#12247=DIRECTION('',(0.,-1.,0.));
#12248=DIRECTION('center_axis',(0.,0.,-1.));
#12249=DIRECTION('ref_axis',(1.,0.,0.));
#12250=DIRECTION('',(-0.688642993486688,0.72510056373009,0.));
#12251=DIRECTION('center_axis',(0.,0.,-1.));
#12252=DIRECTION('ref_axis',(1.,0.,0.));
#12253=DIRECTION('center_axis',(0.,0.,1.));
#12254=DIRECTION('ref_axis',(1.,0.,0.));
#12255=DIRECTION('',(1.,0.,0.));
#12256=DIRECTION('',(1.,0.,0.));
#12257=DIRECTION('',(0.,1.,0.));
#12258=DIRECTION('center_axis',(0.,0.,-1.));
#12259=DIRECTION('ref_axis',(-1.,0.,0.));
#12260=DIRECTION('',(0.688642993486688,-0.72510056373009,0.));
#12261=DIRECTION('center_axis',(0.,0.,-1.));
#12262=DIRECTION('ref_axis',(1.,0.,0.));
#12263=DIRECTION('',(0.,1.,0.));
#12264=DIRECTION('center_axis',(0.,0.,-1.));
#12265=DIRECTION('ref_axis',(1.,0.,0.));
#12266=DIRECTION('center_axis',(0.,0.,-1.));
#12267=DIRECTION('ref_axis',(-1.,0.,0.));
#12268=DIRECTION('',(0.725100563730095,0.688642993486682,0.));
#12269=DIRECTION('',(0.725100563730095,0.688642993486682,0.));
#12270=DIRECTION('',(-0.688642993486682,0.725100563730095,0.));
#12271=DIRECTION('center_axis',(0.,0.,1.));
#12272=DIRECTION('ref_axis',(1.,0.,0.));
#12273=DIRECTION('',(-0.688642993486681,-0.725100563730095,0.));
#12274=DIRECTION('center_axis',(0.,0.,-1.));
#12275=DIRECTION('ref_axis',(1.,-1.73472347597681E-15,0.));
#12276=DIRECTION('center_axis',(0.,0.,-1.));
#12277=DIRECTION('ref_axis',(1.,0.,0.));
#12278=DIRECTION('center_axis',(0.,0.,1.));
#12279=DIRECTION('ref_axis',(1.,0.,0.));
#12280=DIRECTION('',(0.725100563730095,-0.688642993486682,0.));
#12281=DIRECTION('',(0.725100563730095,-0.688642993486682,0.));
#12282=DIRECTION('',(-0.688642993486681,-0.725100563730095,0.));
#12283=DIRECTION('center_axis',(0.,0.,-1.));
#12284=DIRECTION('ref_axis',(-1.,0.,0.));
#12285=DIRECTION('',(0.,-1.,0.));
#12286=DIRECTION('center_axis',(0.,0.,-1.));
#12287=DIRECTION('ref_axis',(1.,-1.73472347597681E-15,0.));
#12288=DIRECTION('',(0.688642993486681,0.725100563730095,0.));
#12289=DIRECTION('center_axis',(0.,0.,-1.));
#12290=DIRECTION('ref_axis',(1.,0.,0.));
#12291=DIRECTION('center_axis',(0.,0.,-1.));
#12292=DIRECTION('ref_axis',(-1.,0.,0.));
#12293=DIRECTION('',(1.,0.,0.));
#12294=DIRECTION('',(1.,0.,0.));
#12295=DIRECTION('center_axis',(0.688642993486682,0.725100563730095,0.));
#12296=DIRECTION('ref_axis',(-0.725100563730095,0.688642993486682,0.));
#12297=DIRECTION('',(0.725100563730095,-0.688642993486682,0.));
#12298=DIRECTION('',(0.,0.,-1.));
#12299=DIRECTION('',(0.,0.,-1.));
#12300=DIRECTION('center_axis',(0.725100563730096,-0.688642993486682,0.));
#12301=DIRECTION('ref_axis',(0.688642993486682,0.725100563730096,0.));
#12302=DIRECTION('',(-0.688642993486681,-0.725100563730095,0.));
#12303=DIRECTION('',(0.,0.,-1.));
#12304=DIRECTION('center_axis',(0.688642993486682,0.725100563730095,0.));
#12305=DIRECTION('ref_axis',(-0.725100563730095,0.688642993486682,0.));
#12306=DIRECTION('',(0.725100563730095,-0.688642993486682,0.));
#12307=DIRECTION('',(0.,0.,-1.));
#12308=DIRECTION('center_axis',(0.,0.,-1.));
#12309=DIRECTION('ref_axis',(-1.,0.,0.));
#12310=DIRECTION('',(0.,0.,-1.));
#12311=DIRECTION('center_axis',(0.,1.,0.));
#12312=DIRECTION('ref_axis',(0.,0.,1.));
#12313=DIRECTION('',(0.,0.,-1.));
#12314=DIRECTION('center_axis',(0.,0.,-1.));
#12315=DIRECTION('ref_axis',(-1.,0.,0.));
#12316=DIRECTION('',(0.,0.,-1.));
#12317=DIRECTION('center_axis',(-0.688642993486682,0.725100563730095,0.));
#12318=DIRECTION('ref_axis',(-0.725100563730095,-0.688642993486682,0.));
#12319=DIRECTION('',(0.,0.,-1.));
#12320=DIRECTION('',(0.725100563730095,0.688642993486682,0.));
#12321=DIRECTION('center_axis',(-0.725100563730095,-0.688642993486682,0.));
#12322=DIRECTION('ref_axis',(0.688642993486682,-0.725100563730095,0.));
#12323=DIRECTION('',(0.,0.,-1.));
#12324=DIRECTION('',(-0.688642993486682,0.725100563730095,0.));
#12325=DIRECTION('center_axis',(-0.688642993486682,0.725100563730095,0.));
#12326=DIRECTION('ref_axis',(-0.725100563730095,-0.688642993486682,0.));
#12327=DIRECTION('',(0.,0.,-1.));
#12328=DIRECTION('',(0.725100563730095,0.688642993486682,0.));
#12329=DIRECTION('center_axis',(0.,0.,-1.));
#12330=DIRECTION('ref_axis',(-1.,0.,0.));
#12331=DIRECTION('',(0.,0.,-1.));
#12332=DIRECTION('center_axis',(0.,1.,0.));
#12333=DIRECTION('ref_axis',(0.,0.,1.));
#12334=DIRECTION('',(0.,0.,-1.));
#12335=DIRECTION('center_axis',(0.,0.,-1.));
#12336=DIRECTION('ref_axis',(-1.,0.,0.));
#12337=DIRECTION('center_axis',(0.,0.,1.));
#12338=DIRECTION('ref_axis',(1.,0.,0.));
#12339=DIRECTION('center_axis',(0.,0.,1.));
#12340=DIRECTION('ref_axis',(1.,0.,0.));
#12341=DIRECTION('axis',(0.,0.,1.));
#12342=DIRECTION('refdir',(1.,0.,0.));
#12343=DIRECTION('axis',(0.,0.,1.));
#12344=DIRECTION('refdir',(1.,0.,0.));
#12345=DIRECTION('axis',(0.,0.,1.));
#12346=DIRECTION('refdir',(1.,0.,0.));
#12347=DIRECTION('center_axis',(0.,-1.,0.));
#12348=DIRECTION('ref_axis',(-1.,0.,4.62458911837273E-15));
#12349=DIRECTION('center_axis',(0.,-1.,0.));
#12350=DIRECTION('ref_axis',(0.,0.,-1.));
#12351=DIRECTION('center_axis',(0.,-1.,0.));
#12352=DIRECTION('ref_axis',(0.,0.,-1.));
#12353=DIRECTION('center_axis',(0.,-1.,0.));
#12354=DIRECTION('ref_axis',(-1.,0.,1.23732655358444E-14));
#12355=DIRECTION('center_axis',(0.743631852678534,0.668589311671889,-2.62185987116465E-14));
#12356=DIRECTION('ref_axis',(0.668589311671889,-0.743631852678534,1.25864554174254E-13));
#12357=DIRECTION('',(0.,-1.,0.));
#12358=DIRECTION('',(0.,1.,0.));
#12359=DIRECTION('center_axis',(-0.939692620785906,0.342020143325676,0.));
#12360=DIRECTION('ref_axis',(0.342020143325676,0.939692620785906,0.));
#12361=DIRECTION('center_axis',(0.,1.,0.));
#12362=DIRECTION('ref_axis',(0.,0.,1.));
#12363=DIRECTION('center_axis',(0.939692620785893,-0.342020143325712,0.));
#12364=DIRECTION('ref_axis',(0.342020143325712,0.939692620785892,0.));
#12365=DIRECTION('center_axis',(0.,1.,0.));
#12366=DIRECTION('ref_axis',(0.,0.,1.));
#12367=DIRECTION('center_axis',(-0.939692620785912,0.342020143325658,0.));
#12368=DIRECTION('ref_axis',(0.342020143325658,0.939692620785912,0.));
#12369=DIRECTION('center_axis',(0.,1.,0.));
#12370=DIRECTION('ref_axis',(0.,0.,1.));
#12371=DIRECTION('center_axis',(0.939692620785903,-0.342020143325684,0.));
#12372=DIRECTION('ref_axis',(0.342020143325684,0.939692620785903,0.));
#12373=DIRECTION('center_axis',(0.,-1.,0.));
#12374=DIRECTION('ref_axis',(0.,0.,-1.));
#12375=DIRECTION('center_axis',(-0.939692620511996,0.342020144078236,8.43754759995423E-9));
#12376=DIRECTION('ref_axis',(0.342020133096614,0.939692590333984,0.000253432399138535));
#12377=DIRECTION('center_axis',(0.,-1.,0.));
#12378=DIRECTION('ref_axis',(0.,0.,-1.));
#12379=DIRECTION('center_axis',(-0.939692620785898,0.342020143325697,0.));
#12380=DIRECTION('ref_axis',(0.342020143325697,0.939692620785898,0.));
#12381=DIRECTION('center_axis',(0.,1.,0.));
#12382=DIRECTION('ref_axis',(0.,0.,1.));
#12383=DIRECTION('center_axis',(0.939692620785645,-0.342020143326393,-2.19010336039703E-11));
#12384=DIRECTION('ref_axis',(0.0107655764198749,0.029578178056861,0.999504494110549));
#12385=DIRECTION('center_axis',(9.02291843310903E-15,-1.,0.));
#12386=DIRECTION('ref_axis',(1.,9.02291843310903E-15,0.));
#12387=DIRECTION('center_axis',(-0.939692620785912,0.34202014332566,0.));
#12388=DIRECTION('ref_axis',(0.34202014332566,0.939692620785912,0.));
#12389=DIRECTION('center_axis',(0.,1.,0.));
#12390=DIRECTION('ref_axis',(0.,0.,1.));
#12391=DIRECTION('center_axis',(0.939692620785907,-0.342020143325674,0.));
#12392=DIRECTION('ref_axis',(0.342020143325674,0.939692620785906,0.));
#12393=DIRECTION('center_axis',(0.,-1.,0.));
#12394=DIRECTION('ref_axis',(0.,0.,-1.));
#12395=DIRECTION('center_axis',(0.,1.,0.));
#12396=DIRECTION('ref_axis',(0.,0.,1.));
#12397=DIRECTION('center_axis',(-0.939692620795782,0.342020143298542,3.39428506811506E-10));
#12398=DIRECTION('ref_axis',(-0.0277714265141323,-0.0763013682495896,0.996697972844638));
#12399=DIRECTION('center_axis',(9.55895934315848E-14,-1.,0.));
#12400=DIRECTION('ref_axis',(1.,9.55895934315848E-14,0.));
#12401=DIRECTION('center_axis',(0.939692620873966,-0.342020143083733,-3.1904885373823E-9));
#12402=DIRECTION('ref_axis',(0.342020143069404,0.939692620834511,9.16256361077704E-6));
#12403=DIRECTION('center_axis',(0.,-1.,0.));
#12404=DIRECTION('ref_axis',(0.,0.,-1.));
#12405=DIRECTION('center_axis',(-0.939692620820882,0.342020143229581,1.5009194657192E-9));
#12406=DIRECTION('ref_axis',(-0.0225366896420474,-0.0619190502992386,0.99782670280466));
#12407=DIRECTION('center_axis',(0.,1.,0.));
#12408=DIRECTION('ref_axis',(0.,0.,1.));
#12409=DIRECTION('center_axis',(0.939692620785924,-0.342020143325626,0.));
#12410=DIRECTION('ref_axis',(0.342020143325626,0.939692620785924,0.));
#12411=DIRECTION('center_axis',(9.02291843310883E-15,-1.,0.));
#12412=DIRECTION('ref_axis',(1.,9.02291843310883E-15,0.));
#12413=DIRECTION('center_axis',(-0.939692620793947,0.342020143303582,3.78133454569351E-10));
#12414=DIRECTION('ref_axis',(-0.0205843228268227,-0.0565549632693089,0.998187267892838));
#12415=DIRECTION('center_axis',(0.,1.,0.));
#12416=DIRECTION('ref_axis',(0.,0.,1.));
#12417=DIRECTION('center_axis',(0.939692621043355,-0.342020142618341,-9.9043275494315E-9));
#12418=DIRECTION('ref_axis',(0.342020142542167,0.93969262083468,-2.10780958412509E-5));
#12419=DIRECTION('center_axis',(-0.939692620785991,0.342020143325442,9.72407375337609E-12));
#12420=DIRECTION('ref_axis',(-0.00753651872272651,-0.0207064150403614,0.999757193153277));
#12421=DIRECTION('center_axis',(0.,1.,0.));
#12422=DIRECTION('ref_axis',(0.,0.,1.));
#12423=DIRECTION('center_axis',(0.939692620786435,-0.342020143324221,-2.68615183328056E-11));
#12424=DIRECTION('ref_axis',(-0.0215495755144781,-0.0592069722035353,0.998013101235467));
#12425=DIRECTION('center_axis',(9.02291843310998E-15,-1.,0.));
#12426=DIRECTION('ref_axis',(1.,9.02291843310998E-15,0.));
#12427=DIRECTION('center_axis',(0.939692620785836,-0.342020143325866,-7.69950011431104E-11));
#12428=DIRECTION('ref_axis',(-1.01602967944146E-8,-2.81402044234508E-8,
1.));
#12429=DIRECTION('center_axis',(8.5216451868249E-15,-1.,0.));
#12430=DIRECTION('ref_axis',(1.,8.5216451868249E-15,0.));
#12431=DIRECTION('center_axis',(-0.939692620782621,0.342020143334701,2.83977188042502E-10));
#12432=DIRECTION('ref_axis',(0.34202014333426,0.93969262078141,-1.60519176623668E-6));
#12433=DIRECTION('center_axis',(0.,1.,0.));
#12434=DIRECTION('ref_axis',(0.,0.,1.));
#12435=DIRECTION('center_axis',(0.939692620775702,-0.34202014335371,-1.52236570283443E-9));
#12436=DIRECTION('ref_axis',(0.342020129216995,0.939692581934119,0.00028752109377726));
#12437=DIRECTION('center_axis',(0.,1.,0.));
#12438=DIRECTION('ref_axis',(0.,0.,1.));
#12439=DIRECTION('center_axis',(-0.939692620780079,0.342020143341686,1.23678408818376E-9));
#12440=DIRECTION('ref_axis',(0.342020143340426,0.939692620776608,2.71743947290395E-6));
#12441=DIRECTION('center_axis',(-0.139173100959747,-0.990268068741615,5.58619456690194E-12));
#12442=DIRECTION('ref_axis',(0.0423831911833703,-0.00595656906061137,0.999083672366904));
#12443=DIRECTION('center_axis',(-0.939692620785275,0.342020143327408,6.43743206976224E-11));
#12444=DIRECTION('ref_axis',(0.00973393684930062,0.0267437715074861,0.99959492853804));
#12445=DIRECTION('center_axis',(0.,1.,0.));
#12446=DIRECTION('ref_axis',(0.,0.,1.));
#12447=DIRECTION('center_axis',(0.939692620786243,-0.342020143324749,-1.75186020081755E-10));
#12448=DIRECTION('ref_axis',(0.342020143324749,0.939692620786243,-1.25974742892378E-8));
#12449=DIRECTION('center_axis',(0.,-1.,0.));
#12450=DIRECTION('ref_axis',(0.,0.,-1.));
#12451=DIRECTION('center_axis',(-0.939692620785062,0.342020143327994,2.78834985027137E-10));
#12452=DIRECTION('ref_axis',(0.342020142367096,0.939692618145078,-7.49589305478533E-5));
#12453=DIRECTION('center_axis',(0.,-1.,0.));
#12454=DIRECTION('ref_axis',(0.,0.,-1.));
#12455=DIRECTION('center_axis',(0.939692620783535,-0.342020143332191,-4.73459073470638E-10));
#12456=DIRECTION('ref_axis',(0.342020143331682,0.939692620782135,1.72597887600438E-6));
#12457=DIRECTION('center_axis',(0.139173100959991,0.990268068741581,-4.68052739465651E-12));
#12458=DIRECTION('ref_axis',(0.0389717259784322,-0.00547711889407729,0.99922530279356));
#12459=DIRECTION('center_axis',(0.,0.,-1.));
#12460=DIRECTION('ref_axis',(-1.,0.,0.));
#12461=DIRECTION('',(0.,0.,-1.));
#12462=DIRECTION('',(0.,0.,-1.));
#12463=DIRECTION('center_axis',(0.,0.,-1.));
#12464=DIRECTION('ref_axis',(-1.,0.,0.));
#12465=DIRECTION('',(0.,0.,-1.));
#12466=DIRECTION('',(0.,0.,-1.));
#12467=DIRECTION('center_axis',(0.,0.,-1.));
#12468=DIRECTION('ref_axis',(-1.,0.,0.));
#12469=DIRECTION('',(0.,0.,-1.));
#12470=DIRECTION('',(0.,0.,-1.));
#12471=DIRECTION('center_axis',(0.,0.,-1.));
#12472=DIRECTION('ref_axis',(-1.,0.,0.));
#12473=DIRECTION('',(0.,0.,-1.));
#12474=DIRECTION('',(0.,0.,-1.));
#12475=DIRECTION('center_axis',(0.,0.,-1.));
#12476=DIRECTION('ref_axis',(-1.,0.,0.));
#12477=DIRECTION('',(0.,0.,-1.));
#12478=DIRECTION('',(0.,0.,-1.));
#12479=DIRECTION('center_axis',(0.,0.,-1.));
#12480=DIRECTION('ref_axis',(-1.,0.,0.));
#12481=DIRECTION('',(0.,0.,-1.));
#12482=DIRECTION('',(0.,0.,-1.));
#12483=DIRECTION('center_axis',(0.,0.,-1.));
#12484=DIRECTION('ref_axis',(-1.,0.,0.));
#12485=DIRECTION('',(0.,0.,-1.));
#12486=DIRECTION('',(0.,0.,-1.));
#12487=DIRECTION('center_axis',(0.,0.,-1.));
#12488=DIRECTION('ref_axis',(-1.,0.,0.));
#12489=DIRECTION('',(0.,0.,-1.));
#12490=DIRECTION('',(0.,0.,-1.));
#12491=DIRECTION('center_axis',(0.,0.,-1.));
#12492=DIRECTION('ref_axis',(-1.,0.,0.));
#12493=DIRECTION('',(0.,0.,-1.));
#12494=DIRECTION('',(0.,0.,-1.));
#12495=DIRECTION('center_axis',(0.,0.,-1.));
#12496=DIRECTION('ref_axis',(-1.,0.,0.));
#12497=DIRECTION('',(0.,0.,-1.));
#12498=DIRECTION('',(0.,0.,-1.));
#12499=DIRECTION('center_axis',(0.,-1.,0.));
#12500=DIRECTION('ref_axis',(0.,0.,-1.));
#12501=DIRECTION('center_axis',(0.,-1.,0.));
#12502=DIRECTION('ref_axis',(0.,0.,-1.));
#12503=DIRECTION('',(0.,-1.,0.));
#12504=DIRECTION('center_axis',(0.,-1.,0.));
#12505=DIRECTION('ref_axis',(0.,0.,-1.));
#12506=DIRECTION('center_axis',(0.,-1.,0.));
#12507=DIRECTION('ref_axis',(-1.,0.,2.60330291914301E-15));
#12508=DIRECTION('center_axis',(0.,-1.,0.));
#12509=DIRECTION('ref_axis',(0.,0.,-1.));
#12510=DIRECTION('center_axis',(0.,-1.,0.));
#12511=DIRECTION('ref_axis',(0.,0.,-1.));
#12512=DIRECTION('center_axis',(0.,-1.,0.));
#12513=DIRECTION('ref_axis',(-1.,0.,-2.02444066332308E-14));
#12514=DIRECTION('',(0.,1.,0.));
#12515=DIRECTION('center_axis',(0.743631852678536,0.668589311671888,3.57157235827042E-16));
#12516=DIRECTION('ref_axis',(0.668589311671888,-0.743631852678536,6.99619203899514E-17));
#12517=DIRECTION('',(0.,-1.,0.));
#12518=DIRECTION('center_axis',(0.,0.,1.));
#12519=DIRECTION('ref_axis',(1.,0.,0.));
#12520=DIRECTION('center_axis',(0.,0.,-1.));
#12521=DIRECTION('ref_axis',(1.,0.,0.));
#12522=DIRECTION('',(0.,0.,1.));
#12523=DIRECTION('center_axis',(0.,0.,-1.));
#12524=DIRECTION('ref_axis',(1.,0.,0.));
#12525=DIRECTION('center_axis',(0.,0.,1.));
#12526=DIRECTION('ref_axis',(1.,0.,0.));
#12527=DIRECTION('center_axis',(0.,0.,1.));
#12528=DIRECTION('ref_axis',(-1.,0.,0.));
#12529=DIRECTION('',(0.,0.,1.));
#12530=DIRECTION('center_axis',(0.,0.,1.));
#12531=DIRECTION('ref_axis',(-1.,0.,0.));
#12532=DIRECTION('center_axis',(0.743631852678536,0.668589311671888,0.));
#12533=DIRECTION('ref_axis',(0.,0.,-1.));
#12534=DIRECTION('',(-0.668589311671888,0.743631852678536,0.));
#12535=DIRECTION('',(0.,0.,-1.));
#12536=DIRECTION('',(-0.668589311671888,0.743631852678536,0.));
#12537=DIRECTION('',(0.668589311671888,-0.743631852678536,0.));
#12538=DIRECTION('',(0.,0.,-1.));
#12539=DIRECTION('',(0.668589311671888,-0.743631852678536,0.));
#12540=DIRECTION('center_axis',(-0.951056516295154,-0.309016994374947,0.));
#12541=DIRECTION('ref_axis',(-0.309016994374947,0.951056516295154,0.));
#12542=DIRECTION('',(0.,0.,-1.));
#12543=DIRECTION('',(-0.309016994374947,0.951056516295154,0.));
#12544=DIRECTION('center_axis',(-0.951056516295158,-0.309016994374935,8.03136146736367E-14));
#12545=DIRECTION('ref_axis',(0.309016994374935,-0.951056516295158,1.03453416570308E-12));
#12546=DIRECTION('',(0.,0.,-1.));
#12547=DIRECTION('center_axis',(-0.951056516295157,-0.309016994374936,-4.45620418678671E-14));
#12548=DIRECTION('ref_axis',(0.309016994374936,-0.951056516295157,-1.10306239593794E-13));
#12549=DIRECTION('',(0.309016994374947,-0.951056516295154,0.));
#12550=DIRECTION('',(0.,0.,-1.));
#12551=DIRECTION('',(0.309016994374947,-0.951056516295154,0.));
#12552=DIRECTION('center_axis',(-0.95105651629528,-0.309016994374559,-1.94886119378061E-13));
#12553=DIRECTION('ref_axis',(0.309016994374559,-0.95105651629528,-4.20853647595452E-13));
#12554=DIRECTION('',(0.,0.,-1.));
#12555=DIRECTION('center_axis',(-0.951056516295095,-0.309016994375127,2.7013917537549E-14));
#12556=DIRECTION('ref_axis',(0.309016994375127,-0.951056516295095,6.64708788606577E-13));
#12557=DIRECTION('',(-0.309016994374947,0.951056516295154,0.));
#12558=DIRECTION('center_axis',(0.,0.,-1.));
#12559=DIRECTION('ref_axis',(-1.,0.,0.));
#12560=DIRECTION('center_axis',(0.,0.,-1.));
#12561=DIRECTION('ref_axis',(1.,0.,0.));
#12562=DIRECTION('center_axis',(0.,0.,-1.));
#12563=DIRECTION('ref_axis',(1.,0.,0.));
#12564=DIRECTION('center_axis',(0.,0.,-1.));
#12565=DIRECTION('ref_axis',(-1.,0.,0.));
#12566=DIRECTION('center_axis',(0.,0.,1.));
#12567=DIRECTION('ref_axis',(-1.,0.,0.));
#12568=DIRECTION('center_axis',(0.,0.,1.));
#12569=DIRECTION('ref_axis',(-1.,0.,0.));
#12570=DIRECTION('center_axis',(0.,-1.,0.));
#12571=DIRECTION('ref_axis',(0.,0.,-1.));
#12572=DIRECTION('',(-1.,0.,0.));
#12573=DIRECTION('',(-1.,0.,0.));
#12574=DIRECTION('center_axis',(-1.,0.,0.));
#12575=DIRECTION('ref_axis',(0.,0.,1.));
#12576=DIRECTION('',(-1.,0.,0.));
#12577=DIRECTION('center_axis',(-1.,0.,0.));
#12578=DIRECTION('ref_axis',(0.,0.,1.));
#12579=DIRECTION('',(-1.,0.,0.));
#12580=DIRECTION('center_axis',(-1.,0.,0.));
#12581=DIRECTION('ref_axis',(0.,0.,1.));
#12582=DIRECTION('',(-1.,0.,0.));
#12583=DIRECTION('',(-1.,0.,0.));
#12584=DIRECTION('center_axis',(-1.,0.,0.));
#12585=DIRECTION('ref_axis',(0.,0.,1.));
#12586=DIRECTION('',(-1.,0.,0.));
#12587=DIRECTION('',(-1.,0.,0.));
#12588=DIRECTION('center_axis',(0.,0.,1.));
#12589=DIRECTION('ref_axis',(1.,0.,0.));
#12590=DIRECTION('center_axis',(0.,0.,-1.));
#12591=DIRECTION('ref_axis',(0.,-1.,0.));
#12592=DIRECTION('center_axis',(0.,-1.,0.));
#12593=DIRECTION('ref_axis',(0.,0.,-1.));
#12594=DIRECTION('center_axis',(0.,0.,-1.));
#12595=DIRECTION('ref_axis',(-1.,0.,0.));
#12596=DIRECTION('',(0.,0.,-1.));
#12597=DIRECTION('',(0.,0.,-1.));
#12598=DIRECTION('center_axis',(0.,-1.,0.));
#12599=DIRECTION('ref_axis',(0.,0.,-1.));
#12600=DIRECTION('center_axis',(0.,1.,0.));
#12601=DIRECTION('ref_axis',(0.,0.,-1.));
#12602=DIRECTION('center_axis',(0.,0.,-1.));
#12603=DIRECTION('ref_axis',(0.857167300701548,0.515038074910994,0.));
#12604=DIRECTION('',(0.,0.,-1.));
#12605=DIRECTION('',(0.,0.,-1.));
#12606=DIRECTION('center_axis',(0.939692620785945,-0.342020143325568,0.));
#12607=DIRECTION('ref_axis',(0.,0.,-1.));
#12608=DIRECTION('center_axis',(-0.939692620757713,0.342020143403136,5.47084737724244E-9));
#12609=DIRECTION('ref_axis',(0.342020143401293,0.939692620752701,-3.26797089302596E-6));
#12610=DIRECTION('center_axis',(0.,0.,-1.));
#12611=DIRECTION('ref_axis',(-1.,0.,0.));
#12612=DIRECTION('',(0.,0.,-1.));
#12613=DIRECTION('',(0.,0.,-1.));
#12614=DIRECTION('center_axis',(0.,0.,-1.));
#12615=DIRECTION('ref_axis',(0.81915204428879,0.573576436351334,0.));
#12616=DIRECTION('',(0.,0.,-1.));
#12617=DIRECTION('',(0.,0.,-1.));
#12618=DIRECTION('center_axis',(0.,0.,-1.));
#12619=DIRECTION('ref_axis',(0.819152044288498,0.573576436351752,0.));
#12620=DIRECTION('',(0.,0.,-1.));
#12621=DIRECTION('',(0.,0.,-1.));
#12622=DIRECTION('center_axis',(-0.939692620785868,0.342020143325781,0.));
#12623=DIRECTION('ref_axis',(0.,0.,1.));
#12624=DIRECTION('',(0.,0.,-1.));
#12625=DIRECTION('center_axis',(0.939692620756647,-0.342020143406064,-2.49208198322954E-9));
#12626=DIRECTION('ref_axis',(0.342020143399459,0.939692620738456,6.22135617963873E-6));
#12627=DIRECTION('center_axis',(0.,1.,0.));
#12628=DIRECTION('ref_axis',(1.,0.,0.));
#12629=DIRECTION('',(0.,0.,-1.));
#12630=DIRECTION('center_axis',(0.,-1.,0.));
#12631=DIRECTION('ref_axis',(0.,0.,1.));
#12632=DIRECTION('center_axis',(0.93969262078596,-0.342020143325527,0.));
#12633=DIRECTION('ref_axis',(0.,0.,-1.));
#12634=DIRECTION('center_axis',(-0.939692620654755,0.34202014368601,1.88817218458711E-8));
#12635=DIRECTION('ref_axis',(0.342020143309401,0.939692619617437,4.69801705537896E-5));
#12636=DIRECTION('center_axis',(0.,0.,-1.));
#12637=DIRECTION('ref_axis',(-1.,0.,0.));
#12638=DIRECTION('',(0.,0.,-1.));
#12639=DIRECTION('',(0.,0.,-1.));
#12640=DIRECTION('center_axis',(0.,1.,0.));
#12641=DIRECTION('ref_axis',(1.,0.,0.));
#12642=DIRECTION('center_axis',(0.,-1.,0.));
#12643=DIRECTION('ref_axis',(0.,0.,1.));
#12644=DIRECTION('center_axis',(-0.939692620785929,0.342020143325613,0.));
#12645=DIRECTION('ref_axis',(0.,0.,1.));
#12646=DIRECTION('center_axis',(0.939692620740706,-0.342020143449862,-9.36193020985306E-9));
#12647=DIRECTION('ref_axis',(0.342020143449752,0.939692620740426,-7.75892961106619E-7));
#12648=DIRECTION('center_axis',(0.,0.,-1.));
#12649=DIRECTION('ref_axis',(0.857167300701951,0.515038074910322,0.));
#12650=DIRECTION('',(0.,0.,-1.));
#12651=DIRECTION('',(0.,0.,-1.));
#12652=DIRECTION('center_axis',(0.,0.,-1.));
#12653=DIRECTION('ref_axis',(-1.,0.,0.));
#12654=DIRECTION('',(0.,0.,-1.));
#12655=DIRECTION('',(0.,0.,-1.));
#12656=DIRECTION('center_axis',(0.939692620785902,-0.342020143325687,0.));
#12657=DIRECTION('ref_axis',(0.,0.,-1.));
#12658=DIRECTION('',(0.,0.,-1.));
#12659=DIRECTION('center_axis',(-0.939692620790632,0.342020143312691,2.72072675189647E-9));
#12660=DIRECTION('ref_axis',(0.34202014331269,0.939692620790629,-7.24251720827429E-8));
#12661=DIRECTION('center_axis',(0.,-1.,0.));
#12662=DIRECTION('ref_axis',(0.,0.,-1.));
#12663=DIRECTION('',(0.,0.,-1.));
#12664=DIRECTION('center_axis',(0.,1.,0.));
#12665=DIRECTION('ref_axis',(0.,0.,-1.));
#12666=DIRECTION('center_axis',(-0.939692620785841,0.342020143325853,0.));
#12667=DIRECTION('ref_axis',(0.,0.,1.));
#12668=DIRECTION('center_axis',(0.93969262072605,-0.342020143490128,-2.00340794851247E-8));
#12669=DIRECTION('ref_axis',(0.342020143480236,0.939692620699313,-7.55083535543581E-6));
#12670=DIRECTION('center_axis',(0.,1.,0.));
#12671=DIRECTION('ref_axis',(1.,0.,0.));
#12672=DIRECTION('center_axis',(0.,-1.,0.));
#12673=DIRECTION('ref_axis',(0.,0.,1.));
#12674=DIRECTION('center_axis',(-0.939692620785858,0.342020143325806,0.));
#12675=DIRECTION('ref_axis',(0.,0.,1.));
#12676=DIRECTION('center_axis',(0.939692620778689,-0.342020143345504,-7.64511527123761E-10));
#12677=DIRECTION('ref_axis',(0.00870136094134712,0.0239067904689136,0.999676323460371));
#12678=DIRECTION('center_axis',(-0.139173100960053,-0.990268068741572,0.));
#12679=DIRECTION('ref_axis',(-0.990268068741572,0.139173100960053,0.));
#12680=DIRECTION('center_axis',(0.139173100958666,0.990268068741767,-2.34229742290568E-11));
#12681=DIRECTION('ref_axis',(0.0731352434197104,-0.0102784881326754,0.997269065423994));
#12682=DIRECTION('center_axis',(8.5216451868249E-15,-1.,0.));
#12683=DIRECTION('ref_axis',(0.,0.,-1.));
#12684=DIRECTION('center_axis',(-8.5216451868249E-15,1.,0.));
#12685=DIRECTION('ref_axis',(1.,8.5216451868249E-15,0.));
#12686=DIRECTION('center_axis',(0.939692620785902,-0.342020143325686,0.));
#12687=DIRECTION('ref_axis',(0.,0.,-1.));
#12688=DIRECTION('center_axis',(-0.939692620785318,0.34202014332729,9.17014605524648E-10));
#12689=DIRECTION('ref_axis',(0.00123016574252725,0.00337984991849099,0.999993531632467));
#12690=DIRECTION('center_axis',(0.139173100960084,0.990268068741568,0.));
#12691=DIRECTION('ref_axis',(0.,0.,-1.));
#12692=DIRECTION('center_axis',(-0.139173100959608,-0.990268068741635,1.99092207355788E-11));
#12693=DIRECTION('ref_axis',(0.0108635901252007,-0.00152677800395377,0.999939823868676));
#12694=DIRECTION('center_axis',(0.,-1.,0.));
#12695=DIRECTION('ref_axis',(0.0424410111766782,0.,0.99909897436155));
#12696=DIRECTION('center_axis',(0.,0.,-1.));
#12697=DIRECTION('ref_axis',(-1.,0.,0.));
#12698=DIRECTION('',(0.,0.,-1.));
#12699=DIRECTION('',(0.,0.,-1.));
#12700=DIRECTION('center_axis',(0.,0.,-1.));
#12701=DIRECTION('ref_axis',(0.819152044288689,0.573576436351479,0.));
#12702=DIRECTION('',(0.,0.,-1.));
#12703=DIRECTION('',(0.,0.,-1.));
#12704=DIRECTION('center_axis',(0.,0.,-1.));
#12705=DIRECTION('ref_axis',(-1.,0.,0.));
#12706=DIRECTION('',(0.,0.,-1.));
#12707=DIRECTION('',(0.,0.,-1.));
#12708=DIRECTION('center_axis',(0.939692620785901,-0.34202014332569,0.));
#12709=DIRECTION('ref_axis',(0.,0.,-1.));
#12710=DIRECTION('center_axis',(-0.939692620791585,0.342020143310072,2.76439098099266E-10));
#12711=DIRECTION('ref_axis',(-0.018779199792196,-0.051595428194235,0.998491488919469));
#12712=DIRECTION('center_axis',(0.,1.,0.));
#12713=DIRECTION('ref_axis',(1.,0.,0.));
#12714=DIRECTION('center_axis',(0.,-1.,0.));
#12715=DIRECTION('ref_axis',(0.,0.,1.));
#12716=DIRECTION('center_axis',(-0.939692620785898,0.342020143325697,0.));
#12717=DIRECTION('ref_axis',(0.,0.,1.));
#12718=DIRECTION('center_axis',(0.939692620787057,-0.342020143322514,-1.21864227387586E-10));
#12719=DIRECTION('ref_axis',(-0.0111653353620459,-0.0306765071443045,0.999467001554168));
#12720=DIRECTION('center_axis',(9.02291843310998E-15,-1.,0.));
#12721=DIRECTION('ref_axis',(0.,0.,-1.));
#12722=DIRECTION('center_axis',(-9.02291843310998E-15,1.,0.));
#12723=DIRECTION('ref_axis',(1.,9.02291843310998E-15,0.));
#12724=DIRECTION('center_axis',(0.,-1.,0.));
#12725=DIRECTION('ref_axis',(0.,0.,-1.));
#12726=DIRECTION('center_axis',(0.,-1.,0.));
#12727=DIRECTION('ref_axis',(0.,0.,1.));
#12728=DIRECTION('center_axis',(-0.939692620793784,0.34202014330403,5.00403671497544E-10));
#12729=DIRECTION('ref_axis',(-0.0148918174945155,-0.0409149337655042,0.999051651300709));
#12730=DIRECTION('center_axis',(0.,1.,0.));
#12731=DIRECTION('ref_axis',(0.,0.,-1.));
#12732=DIRECTION('center_axis',(0.939692620790132,-0.342020143314065,-3.04219561107597E-10));
#12733=DIRECTION('ref_axis',(-0.0150146483884507,-0.0412524082985595,0.999035934860874));
#12734=DIRECTION('center_axis',(0.,1.,0.));
#12735=DIRECTION('ref_axis',(1.,0.,0.));
#12736=DIRECTION('',(0.,0.,-1.));
#12737=DIRECTION('center_axis',(0.,1.,0.));
#12738=DIRECTION('ref_axis',(0.,0.,1.));
#12739=DIRECTION('center_axis',(0.939692620785898,-0.342020143325696,0.));
#12740=DIRECTION('ref_axis',(0.,0.,-1.));
#12741=DIRECTION('center_axis',(0.939692620786911,-0.342020143322915,-6.55090929055045E-11));
#12742=DIRECTION('ref_axis',(-0.016573537540739,-0.0455354203453562,0.998825231633321));
#12743=DIRECTION('',(0.,0.,-1.));
#12744=DIRECTION('center_axis',(0.,0.,-1.));
#12745=DIRECTION('ref_axis',(-1.,0.,0.));
#12746=DIRECTION('',(0.,0.,-1.));
#12747=DIRECTION('center_axis',(0.,-1.,0.));
#12748=DIRECTION('ref_axis',(0.,0.,-1.));
#12749=DIRECTION('center_axis',(0.,-1.,0.));
#12750=DIRECTION('ref_axis',(0.,0.,-1.));
#12751=DIRECTION('',(0.,0.,-1.));
#12752=DIRECTION('center_axis',(0.,0.,-1.));
#12753=DIRECTION('ref_axis',(0.819152044288978,0.573576436351066,0.));
#12754=DIRECTION('',(0.,0.,-1.));
#12755=DIRECTION('center_axis',(-0.939692620785897,0.3420201433257,0.));
#12756=DIRECTION('ref_axis',(0.,0.,1.));
#12757=DIRECTION('center_axis',(-0.93969262078647,0.342020143324126,4.24783801334617E-11));
#12758=DIRECTION('ref_axis',(-0.0123917693876524,-0.0340461067038697,0.999343437797913));
#12759=DIRECTION('',(0.,0.,-1.));
#12760=DIRECTION('center_axis',(0.,0.,-1.));
#12761=DIRECTION('ref_axis',(-1.,0.,0.));
#12762=DIRECTION('center_axis',(0.,-1.,0.));
#12763=DIRECTION('ref_axis',(0.,0.,-1.));
#12764=DIRECTION('center_axis',(0.,0.,-1.));
#12765=DIRECTION('ref_axis',(-1.,0.,0.));
#12766=DIRECTION('',(0.,0.,-1.));
#12767=DIRECTION('',(0.,0.,-1.));
#12768=DIRECTION('center_axis',(0.,0.,-1.));
#12769=DIRECTION('ref_axis',(0.819152044288392,0.573576436351902,0.));
#12770=DIRECTION('',(0.,0.,-1.));
#12771=DIRECTION('',(0.,0.,-1.));
#12772=DIRECTION('center_axis',(0.,0.,-1.));
#12773=DIRECTION('ref_axis',(0.819152044287955,0.573576436352526,0.));
#12774=DIRECTION('',(0.,0.,-1.));
#12775=DIRECTION('',(0.,0.,-1.));
#12776=DIRECTION('center_axis',(-0.939692620785938,0.342020143325588,0.));
#12777=DIRECTION('ref_axis',(0.,0.,1.));
#12778=DIRECTION('',(0.,0.,-1.));
#12779=DIRECTION('center_axis',(0.939692620846122,-0.342020143160232,-2.75362067841349E-9));
#12780=DIRECTION('ref_axis',(-0.0223414512713557,-0.0613826409535316,0.997864234725676));
#12781=DIRECTION('center_axis',(0.,1.,0.));
#12782=DIRECTION('ref_axis',(1.,0.,0.));
#12783=DIRECTION('',(0.,0.,-1.));
#12784=DIRECTION('center_axis',(0.,-1.,0.));
#12785=DIRECTION('ref_axis',(0.,0.,1.));
#12786=DIRECTION('center_axis',(0.939692620785878,-0.342020143325753,0.));
#12787=DIRECTION('ref_axis',(0.,0.,-1.));
#12788=DIRECTION('center_axis',(-0.939692621045191,0.342020142613297,9.64556489440648E-9));
#12789=DIRECTION('ref_axis',(0.342020142608658,0.939692621032591,-5.18204872764276E-6));
#12790=DIRECTION('center_axis',(0.,0.,-1.));
#12791=DIRECTION('ref_axis',(-1.,0.,0.));
#12792=DIRECTION('',(0.,0.,-1.));
#12793=DIRECTION('',(0.,0.,-1.));
#12794=DIRECTION('center_axis',(0.,1.,0.));
#12795=DIRECTION('ref_axis',(1.,0.,0.));
#12796=DIRECTION('center_axis',(0.,-1.,0.));
#12797=DIRECTION('ref_axis',(0.,0.,1.));
#12798=DIRECTION('center_axis',(-0.939692620785897,0.3420201433257,0.));
#12799=DIRECTION('ref_axis',(0.,0.,1.));
#12800=DIRECTION('center_axis',(0.939692620804342,-0.342020143275023,-6.14262807752616E-10));
#12801=DIRECTION('ref_axis',(-0.0310867167549419,-0.0854100541321011,0.995860802870838));
#12802=DIRECTION('center_axis',(0.,0.,-1.));
#12803=DIRECTION('ref_axis',(-1.,0.,0.));
#12804=DIRECTION('',(0.,0.,-1.));
#12805=DIRECTION('',(0.,0.,-1.));
#12806=DIRECTION('center_axis',(9.55895934315848E-14,-1.,0.));
#12807=DIRECTION('ref_axis',(0.,0.,-1.));
#12808=DIRECTION('center_axis',(-9.55895934315848E-14,1.,0.));
#12809=DIRECTION('ref_axis',(1.,9.55895934315848E-14,0.));
#12810=DIRECTION('center_axis',(0.,0.,-1.));
#12811=DIRECTION('ref_axis',(-1.,0.,0.));
#12812=DIRECTION('',(0.,0.,-1.));
#12813=DIRECTION('',(0.,0.,-1.));
#12814=DIRECTION('center_axis',(0.939692620785924,-0.342020143325626,0.));
#12815=DIRECTION('ref_axis',(0.,0.,-1.));
#12816=DIRECTION('center_axis',(-0.939692620785924,0.342020143325626,0.));
#12817=DIRECTION('ref_axis',(0.342020143325626,0.939692620785924,0.));
#12818=DIRECTION('center_axis',(0.,1.,0.));
#12819=DIRECTION('ref_axis',(1.,0.,0.));
#12820=DIRECTION('center_axis',(0.,-1.,0.));
#12821=DIRECTION('ref_axis',(0.,0.,1.));
#12822=DIRECTION('center_axis',(0.939692620785882,-0.342020143325742,0.));
#12823=DIRECTION('ref_axis',(0.,0.,-1.));
#12824=DIRECTION('',(0.,0.,-1.));
#12825=DIRECTION('center_axis',(-0.93969262093867,0.34202014290596,5.35005826976906E-9));
#12826=DIRECTION('ref_axis',(0.342020142887653,0.939692620888535,-1.03317918376429E-5));
#12827=DIRECTION('center_axis',(0.,-1.,0.));
#12828=DIRECTION('ref_axis',(0.,0.,-1.));
#12829=DIRECTION('',(0.,0.,-1.));
#12830=DIRECTION('center_axis',(0.,1.,0.));
#12831=DIRECTION('ref_axis',(0.,0.,-1.));
#12832=DIRECTION('center_axis',(-0.939692620785905,0.342020143325679,0.));
#12833=DIRECTION('ref_axis',(0.,0.,1.));
#12834=DIRECTION('center_axis',(0.939692620820903,-0.342020143229521,-1.45267385393897E-9));
#12835=DIRECTION('ref_axis',(-0.0247993353019933,-0.0681356180176279,0.997367801027252));
#12836=DIRECTION('center_axis',(9.02291843310883E-15,-1.,0.));
#12837=DIRECTION('ref_axis',(0.,0.,-1.));
#12838=DIRECTION('center_axis',(-9.02291843310883E-15,1.,0.));
#12839=DIRECTION('ref_axis',(1.,9.02291843310883E-15,0.));
#12840=DIRECTION('center_axis',(0.,-1.,0.));
#12841=DIRECTION('ref_axis',(0.,0.,-1.));
#12842=DIRECTION('center_axis',(0.,0.,-1.));
#12843=DIRECTION('ref_axis',(-1.,0.,0.));
#12844=DIRECTION('',(0.,0.,-1.));
#12845=DIRECTION('',(0.,0.,-1.));
#12846=DIRECTION('center_axis',(0.,0.,-1.));
#12847=DIRECTION('ref_axis',(0.819152044288572,0.573576436351646,0.));
#12848=DIRECTION('',(0.,0.,-1.));
#12849=DIRECTION('',(0.,0.,-1.));
#12850=DIRECTION('center_axis',(0.,0.,-1.));
#12851=DIRECTION('ref_axis',(0.819152044288157,0.573576436352239,0.));
#12852=DIRECTION('',(0.,0.,-1.));
#12853=DIRECTION('',(0.,0.,-1.));
#12854=DIRECTION('center_axis',(-0.939692620785906,0.342020143325676,0.));
#12855=DIRECTION('ref_axis',(0.,0.,1.));
#12856=DIRECTION('',(0.,0.,-1.));
#12857=DIRECTION('center_axis',(0.939692620785906,-0.342020143325676,0.));
#12858=DIRECTION('ref_axis',(0.342020143325676,0.939692620785906,0.));
#12859=DIRECTION('center_axis',(0.,1.,0.));
#12860=DIRECTION('ref_axis',(1.,0.,0.));
#12861=DIRECTION('',(0.,0.,-1.));
#12862=DIRECTION('center_axis',(0.,-1.,0.));
#12863=DIRECTION('ref_axis',(0.,0.,1.));
#12864=DIRECTION('center_axis',(0.939692620785893,-0.342020143325712,0.));
#12865=DIRECTION('ref_axis',(0.,0.,-1.));
#12866=DIRECTION('center_axis',(-0.939692620785893,0.342020143325712,0.));
#12867=DIRECTION('ref_axis',(0.342020143325712,0.939692620785892,0.));
#12868=DIRECTION('center_axis',(0.,0.,-1.));
#12869=DIRECTION('ref_axis',(-1.,0.,0.));
#12870=DIRECTION('',(0.,0.,-1.));
#12871=DIRECTION('',(0.,0.,-1.));
#12872=DIRECTION('center_axis',(0.,1.,0.));
#12873=DIRECTION('ref_axis',(1.,0.,0.));
#12874=DIRECTION('center_axis',(0.,-1.,0.));
#12875=DIRECTION('ref_axis',(0.,0.,1.));
#12876=DIRECTION('center_axis',(0.939692620785903,-0.342020143325684,0.));
#12877=DIRECTION('ref_axis',(0.,0.,-1.));
#12878=DIRECTION('',(0.,0.,-1.));
#12879=DIRECTION('',(0.,0.,-1.));
#12880=DIRECTION('center_axis',(-0.939692620785903,0.342020143325684,0.));
#12881=DIRECTION('ref_axis',(0.342020143325684,0.939692620785903,0.));
#12882=DIRECTION('center_axis',(0.,-1.,0.));
#12883=DIRECTION('ref_axis',(0.,0.,-1.));
#12884=DIRECTION('',(0.,0.,-1.));
#12885=DIRECTION('center_axis',(0.,1.,0.));
#12886=DIRECTION('ref_axis',(0.,0.,-1.));
#12887=DIRECTION('center_axis',(-0.939692620785938,0.342020143325587,0.));
#12888=DIRECTION('ref_axis',(0.,0.,1.));
#12889=DIRECTION('center_axis',(0.939692620181295,-0.34202014498683,-1.79898375457421E-8));
#12890=DIRECTION('ref_axis',(0.342020144817168,0.939692619716806,-3.14485379223926E-5));
#12891=DIRECTION('center_axis',(-0.939692620785912,0.342020143325658,0.));
#12892=DIRECTION('ref_axis',(0.,0.,1.));
#12893=DIRECTION('',(0.,0.,-1.));
#12894=DIRECTION('center_axis',(0.939692620785912,-0.342020143325658,0.));
#12895=DIRECTION('ref_axis',(0.342020143325658,0.939692620785912,0.));
#12896=DIRECTION('center_axis',(0.,1.,0.));
#12897=DIRECTION('ref_axis',(1.,0.,0.));
#12898=DIRECTION('center_axis',(0.,-1.,0.));
#12899=DIRECTION('ref_axis',(0.,0.,1.));
#12900=DIRECTION('center_axis',(0.,-1.,0.));
#12901=DIRECTION('ref_axis',(0.,0.,-1.));
#12902=DIRECTION('center_axis',(0.,1.,0.));
#12903=DIRECTION('ref_axis',(0.,0.,-1.));
#12904=DIRECTION('center_axis',(0.,-1.,0.));
#12905=DIRECTION('ref_axis',(0.,0.,-1.));
#12906=DIRECTION('center_axis',(0.939692620785907,-0.342020143325674,0.));
#12907=DIRECTION('ref_axis',(0.,0.,-1.));
#12908=DIRECTION('',(0.,0.,-1.));
#12909=DIRECTION('',(0.,0.,-1.));
#12910=DIRECTION('center_axis',(-0.939692620785907,0.342020143325674,0.));
#12911=DIRECTION('ref_axis',(0.342020143325674,0.939692620785907,0.));
#12912=DIRECTION('center_axis',(0.,-1.,0.));
#12913=DIRECTION('ref_axis',(0.,0.,-1.));
#12914=DIRECTION('',(0.,0.,-1.));
#12915=DIRECTION('center_axis',(0.,1.,0.));
#12916=DIRECTION('ref_axis',(0.,0.,-1.));
#12917=DIRECTION('center_axis',(-0.939692620785912,0.34202014332566,0.));
#12918=DIRECTION('ref_axis',(0.,0.,1.));
#12919=DIRECTION('',(0.,0.,-1.));
#12920=DIRECTION('center_axis',(0.939692620785987,-0.342020143325454,-3.76658189380723E-11));
#12921=DIRECTION('ref_axis',(-0.0049092722637038,-0.0134881148006264,0.999896979595881));
#12922=DIRECTION('center_axis',(0.,1.,0.));
#12923=DIRECTION('ref_axis',(1.,0.,0.));
#12924=DIRECTION('center_axis',(0.,-1.,0.));
#12925=DIRECTION('ref_axis',(0.,0.,1.));
#12926=DIRECTION('center_axis',(0.,-1.,0.));
#12927=DIRECTION('ref_axis',(-0.0359601416005055,0.,0.999353224949053));
#12928=DIRECTION('center_axis',(0.939692620785897,-0.3420201433257,0.));
#12929=DIRECTION('ref_axis',(0.,0.,-1.));
#12930=DIRECTION('center_axis',(-0.939692620777725,0.342020143348152,4.80424380319905E-10));
#12931=DIRECTION('ref_axis',(0.0184118528595132,0.0505861485754658,0.998549971331721));
#12932=DIRECTION('center_axis',(0.939692620785639,-0.342020143326409,-1.48599114114919E-11));
#12933=DIRECTION('ref_axis',(0.0156563187134787,0.0430153820934003,0.998951728857656));
#12934=DIRECTION('',(0.,0.,-1.));
#12935=DIRECTION('center_axis',(0.,0.,-1.));
#12936=DIRECTION('ref_axis',(-1.,0.,0.));
#12937=DIRECTION('',(0.,0.,-1.));
#12938=DIRECTION('center_axis',(0.,-1.,0.));
#12939=DIRECTION('ref_axis',(0.,0.,-1.));
#12940=DIRECTION('center_axis',(0.,1.,0.));
#12941=DIRECTION('ref_axis',(0.,0.,-1.));
#12942=DIRECTION('center_axis',(0.,-1.,0.));
#12943=DIRECTION('ref_axis',(0.,0.,-1.));
#12944=DIRECTION('',(0.,0.,-1.));
#12945=DIRECTION('center_axis',(0.,0.,-1.));
#12946=DIRECTION('ref_axis',(0.819152044288933,0.57357643635113,0.));
#12947=DIRECTION('',(0.,0.,-1.));
#12948=DIRECTION('center_axis',(-0.939692620785901,0.34202014332569,0.));
#12949=DIRECTION('ref_axis',(0.,0.,1.));
#12950=DIRECTION('center_axis',(0.939692620773237,-0.342020143360483,-6.51396350366611E-10));
#12951=DIRECTION('ref_axis',(0.0182876877103269,0.0502450071305752,0.99856947666983));
#12952=DIRECTION('center_axis',(-0.939692620784907,0.342020143328419,5.29639891856146E-11));
#12953=DIRECTION('ref_axis',(0.0198804661042492,0.0546211315545426,0.998309220159355));
#12954=DIRECTION('',(0.,0.,-1.));
#12955=DIRECTION('center_axis',(0.,0.,-1.));
#12956=DIRECTION('ref_axis',(-1.,0.,0.));
#12957=DIRECTION('',(0.,0.,-1.));
#12958=DIRECTION('center_axis',(0.,1.,0.));
#12959=DIRECTION('ref_axis',(1.,0.,0.));
#12960=DIRECTION('center_axis',(0.,-1.,0.));
#12961=DIRECTION('ref_axis',(0.,0.,1.));
#12962=DIRECTION('center_axis',(0.,1.,0.));
#12963=DIRECTION('ref_axis',(0.,0.,1.));
#12964=DIRECTION('center_axis',(0.,-1.,0.));
#12965=DIRECTION('ref_axis',(0.,0.,-1.));
#12966=DIRECTION('center_axis',(0.,-1.,0.));
#12967=DIRECTION('ref_axis',(0.,0.,-1.));
#12968=DIRECTION('center_axis',(-0.939692620784216,0.342020143330318,1.32584915794088E-10));
#12969=DIRECTION('ref_axis',(0.0145253292118707,0.0399080136317969,0.999097775625214));
#12970=DIRECTION('center_axis',(0.,-1.,0.));
#12971=DIRECTION('ref_axis',(0.,0.,1.));
#12972=DIRECTION('center_axis',(0.939692620785898,-0.342020143325697,0.));
#12973=DIRECTION('ref_axis',(0.342020143325697,0.939692620785898,0.));
#12974=DIRECTION('center_axis',(-9.02291843310903E-15,1.,0.));
#12975=DIRECTION('ref_axis',(1.,9.02291843310903E-15,0.));
#12976=DIRECTION('center_axis',(0.,1.,0.));
#12977=DIRECTION('ref_axis',(1.,0.,0.));
#12978=DIRECTION('',(0.,0.,-1.));
#12979=DIRECTION('center_axis',(-0.939692620785898,0.342020143325697,0.));
#12980=DIRECTION('ref_axis',(0.,0.,1.));
#12981=DIRECTION('',(0.,0.,-1.));
#12982=DIRECTION('',(0.,0.,-1.));
#12983=DIRECTION('center_axis',(9.02291843310903E-15,-1.,0.));
#12984=DIRECTION('ref_axis',(0.,0.,-1.));
#12985=DIRECTION('',(0.,0.,-1.));
#12986=DIRECTION('',(0.,0.,-1.));
#12987=DIRECTION('center_axis',(0.939692620785925,-0.342020143325624,0.));
#12988=DIRECTION('ref_axis',(0.,0.,-1.));
#12989=DIRECTION('',(0.,0.,-1.));
#12990=DIRECTION('center_axis',(0.,0.,-1.));
#12991=DIRECTION('ref_axis',(-1.,0.,0.));
#12992=DIRECTION('center_axis',(0.,0.,-1.));
#12993=DIRECTION('ref_axis',(0.819152044288523,0.573576436351716,0.));
#12994=DIRECTION('center_axis',(0.,0.,-1.));
#12995=DIRECTION('ref_axis',(-1.,0.,0.));
#12996=DIRECTION('center_axis',(0.,0.,1.));
#12997=DIRECTION('ref_axis',(1.,0.,0.));
#12998=DIRECTION('center_axis',(0.,0.,-1.));
#12999=DIRECTION('ref_axis',(0.,-1.,0.));
#13000=DIRECTION('axis',(0.,0.,1.));
#13001=DIRECTION('refdir',(1.,0.,0.));
#13002=DIRECTION('center_axis',(1.,0.,0.));
#13003=DIRECTION('ref_axis',(0.,0.,-1.));
#13004=DIRECTION('center_axis',(1.,0.,0.));
#13005=DIRECTION('ref_axis',(0.,0.,-1.));
#13006=DIRECTION('center_axis',(0.,1.,1.22464679914735E-16));
#13007=DIRECTION('ref_axis',(0.,-1.22464679914735E-16,1.));
#13008=DIRECTION('center_axis',(1.,0.,0.));
#13009=DIRECTION('ref_axis',(0.,0.,-1.));
#13010=DIRECTION('center_axis',(1.,0.,0.));
#13011=DIRECTION('ref_axis',(0.,0.,-1.));
#13012=DIRECTION('center_axis',(1.,0.,0.));
#13013=DIRECTION('ref_axis',(0.,0.,-1.));
#13014=DIRECTION('',(-1.,0.,0.));
#13015=DIRECTION('center_axis',(1.,0.,0.));
#13016=DIRECTION('ref_axis',(0.,0.,-1.));
#13017=DIRECTION('center_axis',(1.,0.,0.));
#13018=DIRECTION('ref_axis',(0.,0.,-1.));
#13019=DIRECTION('center_axis',(0.,-1.,-1.22464679914735E-16));
#13020=DIRECTION('ref_axis',(0.,-1.22464679914735E-16,1.));
#13021=DIRECTION('center_axis',(1.,0.,0.));
#13022=DIRECTION('ref_axis',(0.,0.,-1.));
#13023=DIRECTION('center_axis',(1.,0.,0.));
#13024=DIRECTION('ref_axis',(0.,0.,-1.));
#13025=DIRECTION('center_axis',(1.,0.,0.));
#13026=DIRECTION('ref_axis',(0.,0.,-1.));
#13027=DIRECTION('',(-1.,0.,0.));
#13028=DIRECTION('center_axis',(1.,0.,0.));
#13029=DIRECTION('ref_axis',(0.,0.,-1.));
#13030=DIRECTION('center_axis',(-1.,0.,0.));
#13031=DIRECTION('ref_axis',(0.,0.,1.));
#13032=DIRECTION('',(0.70710678118655,8.6595605623549E-17,0.707106781186545));
#13033=DIRECTION('center_axis',(1.,0.,0.));
#13034=DIRECTION('ref_axis',(0.,0.,-1.));
#13035=DIRECTION('center_axis',(1.,0.,0.));
#13036=DIRECTION('ref_axis',(0.,0.,-1.));
#13037=DIRECTION('center_axis',(1.,0.,0.));
#13038=DIRECTION('ref_axis',(0.,0.,-1.));
#13039=DIRECTION('center_axis',(1.,0.,0.));
#13040=DIRECTION('ref_axis',(0.,1.,0.));
#13041=DIRECTION('center_axis',(1.,0.,0.));
#13042=DIRECTION('ref_axis',(0.,0.,-1.));
#13043=DIRECTION('center_axis',(1.,0.,0.));
#13044=DIRECTION('ref_axis',(0.,0.,-1.));
#13045=DIRECTION('center_axis',(1.,0.,0.));
#13046=DIRECTION('ref_axis',(0.,0.,-1.));
#13047=DIRECTION('center_axis',(1.,0.,0.));
#13048=DIRECTION('ref_axis',(0.,0.,-1.));
#13049=DIRECTION('center_axis',(1.,0.,0.));
#13050=DIRECTION('ref_axis',(0.,0.,-1.));
#13051=DIRECTION('center_axis',(1.,0.,0.));
#13052=DIRECTION('ref_axis',(0.,0.,-1.));
#13053=DIRECTION('center_axis',(1.,0.,0.));
#13054=DIRECTION('ref_axis',(0.,0.,-1.));
#13055=DIRECTION('center_axis',(1.,0.,0.));
#13056=DIRECTION('ref_axis',(0.,0.,-1.));
#13057=DIRECTION('center_axis',(1.,0.,0.));
#13058=DIRECTION('ref_axis',(0.,0.,-1.));
#13059=DIRECTION('center_axis',(1.,0.,0.));
#13060=DIRECTION('ref_axis',(0.,0.,-1.));
#13061=DIRECTION('center_axis',(0.,0.866025403784439,-0.5));
#13062=DIRECTION('ref_axis',(-1.,0.,0.));
#13063=DIRECTION('',(-1.,0.,0.));
#13064=DIRECTION('',(0.,-0.5,-0.866025403784439));
#13065=DIRECTION('',(-1.,0.,0.));
#13066=DIRECTION('center_axis',(0.,0.866025403784439,0.5));
#13067=DIRECTION('ref_axis',(1.,0.,0.));
#13068=DIRECTION('',(-1.,0.,0.));
#13069=DIRECTION('',(0.,0.5,-0.866025403784439));
#13070=DIRECTION('center_axis',(0.,0.,1.));
#13071=DIRECTION('ref_axis',(1.,0.,0.));
#13072=DIRECTION('',(-1.,0.,0.));
#13073=DIRECTION('',(0.,1.,0.));
#13074=DIRECTION('center_axis',(0.,-0.866025403784439,0.5));
#13075=DIRECTION('ref_axis',(-1.,0.,0.));
#13076=DIRECTION('',(-1.,0.,0.));
#13077=DIRECTION('',(0.,0.5,0.866025403784439));
#13078=DIRECTION('center_axis',(0.,-0.866025403784439,-0.5));
#13079=DIRECTION('ref_axis',(0.,0.5,-0.866025403784439));
#13080=DIRECTION('',(-1.,0.,0.));
#13081=DIRECTION('',(0.,-0.5,0.866025403784439));
#13082=DIRECTION('center_axis',(0.,0.,-1.));
#13083=DIRECTION('ref_axis',(0.,-1.,0.));
#13084=DIRECTION('',(0.,-1.,0.));
#13085=DIRECTION('center_axis',(-1.,0.,0.));
#13086=DIRECTION('ref_axis',(0.,0.,1.));
#13087=DIRECTION('center_axis',(-1.,0.,0.));
#13088=DIRECTION('ref_axis',(0.,0.,1.));
#13089=DIRECTION('center_axis',(-1.,0.,0.));
#13090=DIRECTION('ref_axis',(0.,0.,1.));
#13091=DIRECTION('axis',(0.,0.,1.));
#13092=DIRECTION('refdir',(1.,0.,0.));
#13093=DIRECTION('center_axis',(0.,-1.,0.));
#13094=DIRECTION('ref_axis',(0.,0.,-1.));
#13095=DIRECTION('center_axis',(0.,-1.,0.));
#13096=DIRECTION('ref_axis',(0.,0.,-1.));
#13097=DIRECTION('',(0.,-1.,0.));
#13098=DIRECTION('center_axis',(0.,-1.,0.));
#13099=DIRECTION('ref_axis',(0.,0.,-1.));
#13100=DIRECTION('center_axis',(0.,-1.,0.));
#13101=DIRECTION('ref_axis',(0.,0.,-1.));
#13102=DIRECTION('center_axis',(0.,-1.,0.));
#13103=DIRECTION('ref_axis',(0.,0.,-1.));
#13104=DIRECTION('center_axis',(-1.,0.,-1.22464679914735E-16));
#13105=DIRECTION('ref_axis',(-1.22464679914735E-16,0.,1.));
#13106=DIRECTION('center_axis',(0.,-1.,0.));
#13107=DIRECTION('ref_axis',(0.,0.,-1.));
#13108=DIRECTION('center_axis',(0.,-1.,0.));
#13109=DIRECTION('ref_axis',(0.,0.,-1.));
#13110=DIRECTION('center_axis',(0.,1.,0.));
#13111=DIRECTION('ref_axis',(0.,0.,1.));
#13112=DIRECTION('center_axis',(0.,1.,0.));
#13113=DIRECTION('ref_axis',(0.,0.,1.));
#13114=DIRECTION('center_axis',(0.,1.,0.));
#13115=DIRECTION('ref_axis',(0.,0.,1.));
#13116=DIRECTION('',(4.48815728875744E-17,-0.930423623041689,0.366485854687431));
#13117=DIRECTION('center_axis',(0.,-1.,0.));
#13118=DIRECTION('ref_axis',(0.,0.,-1.));
#13119=DIRECTION('center_axis',(0.,-1.,0.));
#13120=DIRECTION('ref_axis',(0.,0.,1.));
#13121=DIRECTION('',(-9.40548367125564E-17,-0.640430624519258,0.768016025339233));
#13122=DIRECTION('center_axis',(0.,-1.,0.));
#13123=DIRECTION('ref_axis',(0.,0.,-1.));
#13124=DIRECTION('center_axis',(0.,-1.,0.));
#13125=DIRECTION('ref_axis',(0.,0.,-1.));
#13126=DIRECTION('center_axis',(-1.,0.,-1.22464679914735E-16));
#13127=DIRECTION('ref_axis',(-1.22464679914735E-16,0.,1.));
#13128=DIRECTION('center_axis',(0.,-1.,0.));
#13129=DIRECTION('ref_axis',(0.,0.,-1.));
#13130=DIRECTION('center_axis',(0.,-1.,0.));
#13131=DIRECTION('ref_axis',(0.,0.,-1.));
#13132=DIRECTION('center_axis',(0.,-1.,0.));
#13133=DIRECTION('ref_axis',(0.,0.,-1.));
#13134=DIRECTION('',(0.,1.,0.));
#13135=DIRECTION('center_axis',(0.,-1.,0.));
#13136=DIRECTION('ref_axis',(0.,0.,-1.));
#13137=DIRECTION('center_axis',(0.,-1.,0.));
#13138=DIRECTION('ref_axis',(0.,0.,-1.));
#13139=DIRECTION('center_axis',(0.,-1.,0.));
#13140=DIRECTION('ref_axis',(0.,0.,-1.));
#13141=DIRECTION('center_axis',(1.,0.,1.22464679914735E-16));
#13142=DIRECTION('ref_axis',(-1.22464679914735E-16,0.,1.));
#13143=DIRECTION('center_axis',(0.,-1.,0.));
#13144=DIRECTION('ref_axis',(0.,0.,-1.));
#13145=DIRECTION('center_axis',(0.,-1.,0.));
#13146=DIRECTION('ref_axis',(0.,0.,-1.));
#13147=DIRECTION('center_axis',(-1.,0.,-1.22464679914735E-16));
#13148=DIRECTION('ref_axis',(-1.22464679914735E-16,0.,1.));
#13149=DIRECTION('center_axis',(0.,-1.,0.));
#13150=DIRECTION('ref_axis',(0.,0.,-1.));
#13151=DIRECTION('center_axis',(0.,-1.,0.));
#13152=DIRECTION('ref_axis',(0.,0.,-1.));
#13153=DIRECTION('center_axis',(0.,-1.,0.));
#13154=DIRECTION('ref_axis',(0.,0.,-1.));
#13155=DIRECTION('center_axis',(-1.,0.,-1.22464679914735E-16));
#13156=DIRECTION('ref_axis',(-1.22464679914735E-16,0.,1.));
#13157=DIRECTION('center_axis',(0.,-1.,0.));
#13158=DIRECTION('ref_axis',(0.,0.,-1.));
#13159=DIRECTION('center_axis',(0.,-1.,0.));
#13160=DIRECTION('ref_axis',(0.,0.,-1.));
#13161=DIRECTION('center_axis',(0.,1.,0.));
#13162=DIRECTION('ref_axis',(0.,0.,1.));
#13163=DIRECTION('center_axis',(0.,-1.,0.));
#13164=DIRECTION('ref_axis',(0.,0.,-1.));
#13165=DIRECTION('',(-4.18853873767698E-17,0.939692620785909,-0.342020143325668));
#13166=DIRECTION('center_axis',(0.,-1.,0.));
#13167=DIRECTION('ref_axis',(0.,0.,-1.));
#13168=DIRECTION('center_axis',(0.,-1.,0.));
#13169=DIRECTION('ref_axis',(0.,0.,-1.));
#13170=DIRECTION('center_axis',(1.,0.,1.22464679914735E-16));
#13171=DIRECTION('ref_axis',(-1.22464679914735E-16,0.,1.));
#13172=DIRECTION('center_axis',(0.,-1.,0.));
#13173=DIRECTION('ref_axis',(0.,0.,-1.));
#13174=DIRECTION('center_axis',(0.,-1.,0.));
#13175=DIRECTION('ref_axis',(0.,0.,-1.));
#13176=DIRECTION('center_axis',(-1.,0.,-1.22464679914735E-16));
#13177=DIRECTION('ref_axis',(-1.22464679914735E-16,0.,1.));
#13178=DIRECTION('center_axis',(0.,1.,0.));
#13179=DIRECTION('ref_axis',(1.,0.,0.));
#13180=DIRECTION('center_axis',(0.,1.,0.));
#13181=DIRECTION('ref_axis',(1.,0.,0.));
#13182=DIRECTION('center_axis',(0.,-1.,0.));
#13183=DIRECTION('ref_axis',(0.,0.,-1.));
#13184=DIRECTION('center_axis',(0.,-1.,0.));
#13185=DIRECTION('ref_axis',(0.,0.,-1.));
#13186=DIRECTION('center_axis',(0.,1.,0.));
#13187=DIRECTION('ref_axis',(1.,0.,0.));
#13188=DIRECTION('axis',(0.,0.,1.));
#13189=DIRECTION('refdir',(1.,0.,0.));
#13190=DIRECTION('center_axis',(1.,0.,0.));
#13191=DIRECTION('ref_axis',(0.,0.,-1.));
#13192=DIRECTION('center_axis',(1.,0.,0.));
#13193=DIRECTION('ref_axis',(0.,0.,-1.));
#13194=DIRECTION('',(-1.,0.,0.));
#13195=DIRECTION('center_axis',(1.,0.,0.));
#13196=DIRECTION('ref_axis',(0.,0.,-1.));
#13197=DIRECTION('center_axis',(1.,0.,0.));
#13198=DIRECTION('ref_axis',(0.,0.,-1.));
#13199=DIRECTION('center_axis',(1.,0.,0.));
#13200=DIRECTION('ref_axis',(0.,0.,-1.));
#13201=DIRECTION('center_axis',(1.,0.,0.));
#13202=DIRECTION('ref_axis',(0.,0.,-1.));
#13203=DIRECTION('center_axis',(1.,0.,0.));
#13204=DIRECTION('ref_axis',(0.,0.,-1.));
#13205=DIRECTION('center_axis',(1.,0.,0.));
#13206=DIRECTION('ref_axis',(0.,0.,-1.));
#13207=DIRECTION('center_axis',(-1.,0.,0.));
#13208=DIRECTION('ref_axis',(0.,0.,1.));
#13209=DIRECTION('center_axis',(1.,0.,0.));
#13210=DIRECTION('ref_axis',(0.,0.,-1.));
#13211=DIRECTION('',(-0.707106781186548,-8.65956056235493E-17,-0.707106781186547));
#13212=DIRECTION('center_axis',(1.,0.,0.));
#13213=DIRECTION('ref_axis',(0.,0.,-1.));
#13214=DIRECTION('center_axis',(1.,0.,0.));
#13215=DIRECTION('ref_axis',(0.,0.,-1.));
#13216=DIRECTION('center_axis',(1.,0.,0.));
#13217=DIRECTION('ref_axis',(0.,0.,-1.));
#13218=DIRECTION('',(1.,0.,0.));
#13219=DIRECTION('center_axis',(1.,0.,0.));
#13220=DIRECTION('ref_axis',(0.,0.,-1.));
#13221=DIRECTION('center_axis',(1.,0.,0.));
#13222=DIRECTION('ref_axis',(0.,0.,-1.));
#13223=DIRECTION('',(0.707106781186547,-8.65956056235494E-17,0.707106781186548));
#13224=DIRECTION('center_axis',(1.,0.,0.));
#13225=DIRECTION('ref_axis',(0.,0.,-1.));
#13226=DIRECTION('center_axis',(1.,0.,0.));
#13227=DIRECTION('ref_axis',(0.,0.,-1.));
#13228=DIRECTION('center_axis',(1.,0.,0.));
#13229=DIRECTION('ref_axis',(0.,0.,-1.));
#13230=DIRECTION('center_axis',(1.,0.,0.));
#13231=DIRECTION('ref_axis',(0.,1.,0.));
#13232=DIRECTION('center_axis',(1.,0.,0.));
#13233=DIRECTION('ref_axis',(0.,0.,-1.));
#13234=DIRECTION('center_axis',(1.,0.,0.));
#13235=DIRECTION('ref_axis',(0.,0.,-1.));
#13236=DIRECTION('center_axis',(1.,0.,0.));
#13237=DIRECTION('ref_axis',(0.,0.,-1.));
#13238=DIRECTION('center_axis',(1.,0.,0.));
#13239=DIRECTION('ref_axis',(0.,0.,-1.));
#13240=DIRECTION('center_axis',(1.,0.,0.));
#13241=DIRECTION('ref_axis',(0.,0.,-1.));
#13242=DIRECTION('center_axis',(1.,0.,0.));
#13243=DIRECTION('ref_axis',(0.,0.,-1.));
#13244=DIRECTION('center_axis',(1.,0.,0.));
#13245=DIRECTION('ref_axis',(0.,0.,-1.));
#13246=DIRECTION('center_axis',(1.,0.,0.));
#13247=DIRECTION('ref_axis',(0.,0.,-1.));
#13248=DIRECTION('center_axis',(1.,0.,0.));
#13249=DIRECTION('ref_axis',(0.,0.,-1.));
#13250=DIRECTION('center_axis',(1.,0.,0.));
#13251=DIRECTION('ref_axis',(0.,0.,-1.));
#13252=DIRECTION('center_axis',(0.,0.866025403784439,-0.5));
#13253=DIRECTION('ref_axis',(-1.,0.,0.));
#13254=DIRECTION('',(-1.,0.,0.));
#13255=DIRECTION('',(0.,-0.5,-0.866025403784439));
#13256=DIRECTION('',(0.,-0.5,-0.866025403784439));
#13257=DIRECTION('',(-1.,0.,0.));
#13258=DIRECTION('center_axis',(0.,0.866025403784439,0.5));
#13259=DIRECTION('ref_axis',(1.,0.,0.));
#13260=DIRECTION('',(-1.,0.,0.));
#13261=DIRECTION('',(0.,0.5,-0.866025403784439));
#13262=DIRECTION('',(0.,0.5,-0.866025403784439));
#13263=DIRECTION('center_axis',(0.,0.,1.));
#13264=DIRECTION('ref_axis',(1.,0.,0.));
#13265=DIRECTION('',(-1.,0.,0.));
#13266=DIRECTION('',(0.,1.,0.));
#13267=DIRECTION('',(0.,1.,0.));
#13268=DIRECTION('center_axis',(0.,-0.866025403784439,0.5));
#13269=DIRECTION('ref_axis',(-1.,0.,0.));
#13270=DIRECTION('',(-1.,0.,0.));
#13271=DIRECTION('',(0.,0.5,0.866025403784439));
#13272=DIRECTION('',(0.,0.5,0.866025403784439));
#13273=DIRECTION('center_axis',(0.,-0.866025403784439,-0.5));
#13274=DIRECTION('ref_axis',(0.,0.5,-0.866025403784439));
#13275=DIRECTION('',(-1.,0.,0.));
#13276=DIRECTION('',(0.,-0.5,0.866025403784439));
#13277=DIRECTION('',(0.,-0.5,0.866025403784439));
#13278=DIRECTION('center_axis',(0.,0.,-1.));
#13279=DIRECTION('ref_axis',(0.,-1.,0.));
#13280=DIRECTION('',(0.,-1.,0.));
#13281=DIRECTION('',(0.,-1.,0.));
#13282=DIRECTION('center_axis',(-1.,0.,0.));
#13283=DIRECTION('ref_axis',(0.,0.,1.));
#13284=DIRECTION('center_axis',(-1.,0.,0.));
#13285=DIRECTION('ref_axis',(0.,0.,1.));
#13286=DIRECTION('center_axis',(-1.,0.,0.));
#13287=DIRECTION('ref_axis',(0.,0.,1.));
#13288=DIRECTION('center_axis',(-1.,0.,0.));
#13289=DIRECTION('ref_axis',(0.,0.,1.));
#13290=DIRECTION('center_axis',(-1.,0.,0.));
#13291=DIRECTION('ref_axis',(0.,0.,1.));
#13292=DIRECTION('center_axis',(-1.,0.,0.));
#13293=DIRECTION('ref_axis',(0.,0.,1.));
#13294=DIRECTION('center_axis',(-1.,0.,0.));
#13295=DIRECTION('ref_axis',(0.,0.,1.));
#13296=DIRECTION('axis',(0.,0.,1.));
#13297=DIRECTION('refdir',(1.,0.,0.));
#13298=DIRECTION('center_axis',(1.,0.,0.));
#13299=DIRECTION('ref_axis',(0.,0.,-1.));
#13300=DIRECTION('center_axis',(0.,-0.707106781186547,0.707106781186548));
#13301=DIRECTION('ref_axis',(1.,0.,0.));
#13302=DIRECTION('center_axis',(1.,1.3055303676213E-17,0.));
#13303=DIRECTION('ref_axis',(1.3055303676213E-17,-1.,0.));
#13304=DIRECTION('center_axis',(1.,1.3055303676213E-17,0.));
#13305=DIRECTION('ref_axis',(1.3055303676213E-17,-1.,0.));
#13306=DIRECTION('center_axis',(0.,-0.707106781186547,-0.707106781186548));
#13307=DIRECTION('ref_axis',(1.,0.,0.));
#13308=DIRECTION('center_axis',(-1.,-1.3055303676213E-17,0.));
#13309=DIRECTION('ref_axis',(1.3055303676213E-17,-1.,0.));
#13310=DIRECTION('center_axis',(1.,1.3055303676213E-17,0.));
#13311=DIRECTION('ref_axis',(-1.3055303676213E-17,1.,0.));
#13312=DIRECTION('center_axis',(1.,1.3055303676213E-17,0.));
#13313=DIRECTION('ref_axis',(-1.3055303676213E-17,1.,0.));
#13314=DIRECTION('',(-0.707106781186553,0.707106781186542,8.65956056235486E-17));
#13315=DIRECTION('',(-0.707106781186551,-0.499999999999998,-0.499999999999998));
#13316=DIRECTION('center_axis',(1.,1.3055303676213E-17,0.));
#13317=DIRECTION('ref_axis',(-1.3055303676213E-17,1.,0.));
#13318=DIRECTION('',(-0.707106781186551,0.499999999999998,-0.499999999999998));
#13319=DIRECTION('center_axis',(1.,1.3055303676213E-17,0.));
#13320=DIRECTION('ref_axis',(-1.3055303676213E-17,1.,0.));
#13321=DIRECTION('center_axis',(1.,1.3055303676213E-17,0.));
#13322=DIRECTION('ref_axis',(-1.3055303676213E-17,1.,0.));
#13323=DIRECTION('',(-0.707106781186547,0.707106781186548,8.65956056235494E-17));
#13324=DIRECTION('center_axis',(1.,1.3055303676213E-17,0.));
#13325=DIRECTION('ref_axis',(-1.3055303676213E-17,1.,0.));
#13326=DIRECTION('center_axis',(1.,1.3055303676213E-17,0.));
#13327=DIRECTION('ref_axis',(-1.3055303676213E-17,1.,0.));
#13328=DIRECTION('center_axis',(1.,1.3055303676213E-17,0.));
#13329=DIRECTION('ref_axis',(-1.3055303676213E-17,1.,0.));
#13330=DIRECTION('',(-1.,-1.3055303676213E-17,0.));
#13331=DIRECTION('center_axis',(1.,1.3055303676213E-17,0.));
#13332=DIRECTION('ref_axis',(0.,1.,0.));
#13333=DIRECTION('center_axis',(1.,1.3055303676213E-17,0.));
#13334=DIRECTION('ref_axis',(-1.3055303676213E-17,1.,0.));
#13335=DIRECTION('center_axis',(1.59881358589709E-33,-1.22464679914735E-16,
1.));
#13336=DIRECTION('ref_axis',(0.,-1.,-1.22464679914735E-16));
#13337=DIRECTION('center_axis',(1.,1.3055303676213E-17,0.));
#13338=DIRECTION('ref_axis',(-1.3055303676213E-17,1.,0.));
#13339=DIRECTION('center_axis',(1.,1.3055303676213E-17,0.));
#13340=DIRECTION('ref_axis',(-1.3055303676213E-17,1.,0.));
#13341=DIRECTION('center_axis',(1.,1.3055303676213E-17,0.));
#13342=DIRECTION('ref_axis',(-1.3055303676213E-17,1.,0.));
#13343=DIRECTION('',(-1.,-1.3055303676213E-17,0.));
#13344=DIRECTION('center_axis',(1.,1.3055303676213E-17,0.));
#13345=DIRECTION('ref_axis',(-1.3055303676213E-17,1.,0.));
#13346=DIRECTION('center_axis',(1.,1.3055303676213E-17,0.));
#13347=DIRECTION('ref_axis',(-1.3055303676213E-17,1.,0.));
#13348=DIRECTION('',(-1.,-1.3055303676213E-17,0.));
#13349=DIRECTION('center_axis',(1.,1.3055303676213E-17,0.));
#13350=DIRECTION('ref_axis',(0.,1.,0.));
#13351=DIRECTION('center_axis',(1.,1.3055303676213E-17,0.));
#13352=DIRECTION('ref_axis',(-1.3055303676213E-17,1.,0.));
#13353=DIRECTION('center_axis',(1.59881358589709E-33,-1.22464679914735E-16,
1.));
#13354=DIRECTION('ref_axis',(0.,-1.,-1.22464679914735E-16));
#13355=DIRECTION('center_axis',(1.,1.3055303676213E-17,0.));
#13356=DIRECTION('ref_axis',(-1.3055303676213E-17,1.,0.));
#13357=DIRECTION('center_axis',(1.,1.3055303676213E-17,0.));
#13358=DIRECTION('ref_axis',(-1.3055303676213E-17,1.,0.));
#13359=DIRECTION('center_axis',(1.,1.3055303676213E-17,0.));
#13360=DIRECTION('ref_axis',(-1.3055303676213E-17,1.,0.));
#13361=DIRECTION('',(-1.,-1.3055303676213E-17,0.));
#13362=DIRECTION('center_axis',(1.,1.3055303676213E-17,0.));
#13363=DIRECTION('ref_axis',(-1.3055303676213E-17,1.,0.));
#13364=DIRECTION('center_axis',(-1.,-1.3055303676213E-17,0.));
#13365=DIRECTION('ref_axis',(1.3055303676213E-17,-1.,0.));
#13366=DIRECTION('',(0.707106781186549,-0.707106781186547,8.65956056235492E-17));
#13367=DIRECTION('center_axis',(1.,1.3055303676213E-17,0.));
#13368=DIRECTION('ref_axis',(-1.3055303676213E-17,1.,0.));
#13369=DIRECTION('center_axis',(1.,1.3055303676213E-17,0.));
#13370=DIRECTION('ref_axis',(0.,1.,0.));
#13371=DIRECTION('center_axis',(1.,1.3055303676213E-17,0.));
#13372=DIRECTION('ref_axis',(-1.3055303676213E-17,1.,0.));
#13373=DIRECTION('center_axis',(1.59881358589709E-33,-1.22464679914735E-16,
1.));
#13374=DIRECTION('ref_axis',(0.,-1.,-1.22464679914735E-16));
#13375=DIRECTION('center_axis',(1.,1.3055303676213E-17,0.));
#13376=DIRECTION('ref_axis',(-1.3055303676213E-17,1.,0.));
#13377=DIRECTION('center_axis',(1.,1.3055303676213E-17,0.));
#13378=DIRECTION('ref_axis',(-1.3055303676213E-17,1.,0.));
#13379=DIRECTION('center_axis',(1.,1.3055303676213E-17,0.));
#13380=DIRECTION('ref_axis',(-1.3055303676213E-17,1.,0.));
#13381=DIRECTION('',(-1.,-1.3055303676213E-17,0.));
#13382=DIRECTION('center_axis',(1.,1.3055303676213E-17,0.));
#13383=DIRECTION('ref_axis',(-1.3055303676213E-17,1.,0.));
#13384=DIRECTION('center_axis',(1.,1.3055303676213E-17,0.));
#13385=DIRECTION('ref_axis',(-1.3055303676213E-17,1.,0.));
#13386=DIRECTION('',(-0.621657859564011,0.783288903050651,9.59252247928621E-17));
#13387=DIRECTION('center_axis',(0.,-0.707106781186547,0.707106781186548));
#13388=DIRECTION('ref_axis',(-1.,0.,0.));
#13389=DIRECTION('',(9.2314937598999E-18,-0.707106781186548,-0.707106781186547));
#13390=DIRECTION('center_axis',(0.,-0.707106781186547,-0.707106781186548));
#13391=DIRECTION('ref_axis',(0.,-0.707106781186548,0.707106781186547));
#13392=DIRECTION('',(-9.2314937598999E-18,0.707106781186548,-0.707106781186547));
#13393=DIRECTION('center_axis',(-1.,-1.3055303676213E-17,0.));
#13394=DIRECTION('ref_axis',(-1.3055303676213E-17,1.,0.));
#13395=DIRECTION('center_axis',(-1.,-1.3055303676213E-17,0.));
#13396=DIRECTION('ref_axis',(-1.3055303676213E-17,1.,0.));
#13397=DIRECTION('center_axis',(1.,1.3055303676213E-17,0.));
#13398=DIRECTION('ref_axis',(-1.3055303676213E-17,1.,0.));
#13399=DIRECTION('center_axis',(-1.,-1.3055303676213E-17,0.));
#13400=DIRECTION('ref_axis',(-1.3055303676213E-17,1.,0.));
#13401=DIRECTION('center_axis',(1.,1.3055303676213E-17,0.));
#13402=DIRECTION('ref_axis',(-1.3055303676213E-17,1.,0.));
#13403=DIRECTION('center_axis',(1.,1.3055303676213E-17,0.));
#13404=DIRECTION('ref_axis',(-1.3055303676213E-17,1.,0.));
#13405=DIRECTION('axis',(0.,0.,1.));
#13406=DIRECTION('refdir',(1.,0.,0.));
#13407=DIRECTION('center_axis',(0.,-1.,0.));
#13408=DIRECTION('ref_axis',(0.,0.,-1.));
#13409=DIRECTION('center_axis',(0.,-1.,0.));
#13410=DIRECTION('ref_axis',(0.,0.,-1.));
#13411=DIRECTION('center_axis',(-1.,0.,-1.22464679914735E-16));
#13412=DIRECTION('ref_axis',(-1.22464679914735E-16,0.,1.));
#13413=DIRECTION('center_axis',(0.,1.,0.));
#13414=DIRECTION('ref_axis',(0.,0.,1.));
#13415=DIRECTION('center_axis',(0.,-1.,0.));
#13416=DIRECTION('ref_axis',(0.,0.,-1.));
#13417=DIRECTION('center_axis',(0.,-1.,0.));
#13418=DIRECTION('ref_axis',(0.,0.,-1.));
#13419=DIRECTION('center_axis',(0.,-1.,0.));
#13420=DIRECTION('ref_axis',(0.,0.,-1.));
#13421=DIRECTION('center_axis',(1.,0.,1.22464679914735E-16));
#13422=DIRECTION('ref_axis',(-1.22464679914735E-16,0.,1.));
#13423=DIRECTION('center_axis',(0.,-1.,0.));
#13424=DIRECTION('ref_axis',(0.,0.,-1.));
#13425=DIRECTION('center_axis',(0.,-1.,0.));
#13426=DIRECTION('ref_axis',(0.,0.,-1.));
#13427=DIRECTION('',(0.,-1.,0.));
#13428=DIRECTION('center_axis',(0.,-1.,0.));
#13429=DIRECTION('ref_axis',(0.,0.,-1.));
#13430=DIRECTION('center_axis',(0.,-1.,0.));
#13431=DIRECTION('ref_axis',(0.,0.,-1.));
#13432=DIRECTION('center_axis',(0.,-1.,0.));
#13433=DIRECTION('ref_axis',(0.,0.,-1.));
#13434=DIRECTION('center_axis',(-1.,0.,-1.22464679914735E-16));
#13435=DIRECTION('ref_axis',(-1.22464679914735E-16,0.,1.));
#13436=DIRECTION('center_axis',(0.,-1.,0.));
#13437=DIRECTION('ref_axis',(0.,0.,-1.));
#13438=DIRECTION('center_axis',(0.,-1.,0.));
#13439=DIRECTION('ref_axis',(0.,0.,-1.));
#13440=DIRECTION('center_axis',(0.,1.,0.));
#13441=DIRECTION('ref_axis',(0.,0.,1.));
#13442=DIRECTION('',(7.98432677834137E-17,-0.758244969689014,0.651969758456101));
#13443=DIRECTION('center_axis',(0.,-1.,0.));
#13444=DIRECTION('ref_axis',(0.,0.,-1.));
#13445=DIRECTION('center_axis',(1.,0.,1.22464679914735E-16));
#13446=DIRECTION('ref_axis',(-1.22464679914735E-16,0.,1.));
#13447=DIRECTION('center_axis',(0.,-1.,0.));
#13448=DIRECTION('ref_axis',(0.,0.,-1.));
#13449=DIRECTION('center_axis',(0.,-1.,0.));
#13450=DIRECTION('ref_axis',(0.,0.,-1.));
#13451=DIRECTION('center_axis',(-1.,0.,-1.22464679914735E-16));
#13452=DIRECTION('ref_axis',(-1.22464679914735E-16,0.,1.));
#13453=DIRECTION('center_axis',(0.,-1.,0.));
#13454=DIRECTION('ref_axis',(0.,0.,-1.));
#13455=DIRECTION('center_axis',(0.,-1.,0.));
#13456=DIRECTION('ref_axis',(0.,0.,-1.));
#13457=DIRECTION('center_axis',(0.,-1.,0.));
#13458=DIRECTION('ref_axis',(0.,0.,-1.));
#13459=DIRECTION('center_axis',(1.,0.,1.22464679914735E-16));
#13460=DIRECTION('ref_axis',(-1.22464679914735E-16,0.,1.));
#13461=DIRECTION('center_axis',(0.,-1.,0.));
#13462=DIRECTION('ref_axis',(0.,0.,-1.));
#13463=DIRECTION('center_axis',(0.,-1.,0.));
#13464=DIRECTION('ref_axis',(0.,0.,-1.));
#13465=DIRECTION('center_axis',(-1.,0.,-1.22464679914735E-16));
#13466=DIRECTION('ref_axis',(-1.22464679914735E-16,0.,1.));
#13467=DIRECTION('center_axis',(0.,-1.,0.));
#13468=DIRECTION('ref_axis',(0.,0.,-1.));
#13469=DIRECTION('center_axis',(0.,-1.,0.));
#13470=DIRECTION('ref_axis',(0.,0.,-1.));
#13471=DIRECTION('center_axis',(0.,1.,0.));
#13472=DIRECTION('ref_axis',(0.,0.,1.));
#13473=DIRECTION('center_axis',(0.,-1.,0.));
#13474=DIRECTION('ref_axis',(0.,0.,-1.));
#13475=DIRECTION('',(-6.10475930061065E-17,0.866894628860328,-0.49849142665959));
#13476=DIRECTION('center_axis',(0.,-1.,0.));
#13477=DIRECTION('ref_axis',(0.,0.,-1.));
#13478=DIRECTION('center_axis',(0.,-1.,0.));
#13479=DIRECTION('ref_axis',(0.,0.,-1.));
#13480=DIRECTION('center_axis',(1.,0.,1.22464679914735E-16));
#13481=DIRECTION('ref_axis',(-1.22464679914735E-16,0.,1.));
#13482=DIRECTION('center_axis',(0.,-1.,0.));
#13483=DIRECTION('ref_axis',(0.,0.,-1.));
#13484=DIRECTION('center_axis',(0.923879532511287,0.,-0.38268343236509));
#13485=DIRECTION('ref_axis',(0.,-1.,0.));
#13486=DIRECTION('',(0.38268343236509,0.,0.923879532511287));
#13487=DIRECTION('',(0.,-1.,0.));
#13488=DIRECTION('',(-0.38268343236509,0.,-0.923879532511287));
#13489=DIRECTION('',(0.,-1.,0.));
#13490=DIRECTION('center_axis',(0.38268343236509,0.,-0.923879532511287));
#13491=DIRECTION('ref_axis',(0.,-1.,0.));
#13492=DIRECTION('',(0.923879532511287,0.,0.38268343236509));
#13493=DIRECTION('',(0.,-1.,0.));
#13494=DIRECTION('',(-0.923879532511287,0.,-0.38268343236509));
#13495=DIRECTION('center_axis',(-0.38268343236509,0.,-0.923879532511287));
#13496=DIRECTION('ref_axis',(-0.923879532511287,0.,0.38268343236509));
#13497=DIRECTION('',(0.923879532511287,0.,-0.38268343236509));
#13498=DIRECTION('',(0.,-1.,0.));
#13499=DIRECTION('',(-0.923879532511287,0.,0.38268343236509));
#13500=DIRECTION('center_axis',(-0.923879532511287,0.,-0.38268343236509));
#13501=DIRECTION('ref_axis',(-0.38268343236509,0.,0.923879532511287));
#13502=DIRECTION('',(0.38268343236509,0.,-0.923879532511287));
#13503=DIRECTION('',(0.,-1.,0.));
#13504=DIRECTION('',(-0.38268343236509,0.,0.923879532511287));
#13505=DIRECTION('center_axis',(-0.923879532511287,0.,0.38268343236509));
#13506=DIRECTION('ref_axis',(0.,1.,0.));
#13507=DIRECTION('',(-0.38268343236509,0.,-0.923879532511287));
#13508=DIRECTION('',(0.,-1.,0.));
#13509=DIRECTION('',(0.38268343236509,0.,0.923879532511287));
#13510=DIRECTION('center_axis',(-0.38268343236509,0.,0.923879532511287));
#13511=DIRECTION('ref_axis',(0.,1.,0.));
#13512=DIRECTION('',(-0.923879532511287,0.,-0.38268343236509));
#13513=DIRECTION('',(0.,-1.,0.));
#13514=DIRECTION('',(0.923879532511287,0.,0.38268343236509));
#13515=DIRECTION('center_axis',(0.38268343236509,0.,0.923879532511287));
#13516=DIRECTION('ref_axis',(0.,-1.,0.));
#13517=DIRECTION('',(-0.923879532511287,0.,0.38268343236509));
#13518=DIRECTION('',(0.,-1.,0.));
#13519=DIRECTION('',(0.923879532511287,0.,-0.38268343236509));
#13520=DIRECTION('center_axis',(0.923879532511287,0.,0.38268343236509));
#13521=DIRECTION('ref_axis',(0.,-1.,0.));
#13522=DIRECTION('',(-0.38268343236509,0.,0.923879532511287));
#13523=DIRECTION('',(0.38268343236509,0.,-0.923879532511287));
#13524=DIRECTION('center_axis',(0.,1.,0.));
#13525=DIRECTION('ref_axis',(1.,0.,0.));
#13526=DIRECTION('center_axis',(0.,-1.,0.));
#13527=DIRECTION('ref_axis',(0.,0.,-1.));
#13528=DIRECTION('center_axis',(0.,-1.,0.));
#13529=DIRECTION('ref_axis',(0.,0.,-1.));
#13530=DIRECTION('center_axis',(0.,1.,0.));
#13531=DIRECTION('ref_axis',(1.,0.,0.));
#13532=DIRECTION('axis',(0.,0.,1.));
#13533=DIRECTION('refdir',(1.,0.,0.));
#13534=DIRECTION('center_axis',(0.,0.,-1.));
#13535=DIRECTION('ref_axis',(-1.,0.,0.));
#13536=DIRECTION('center_axis',(0.,0.,-1.));
#13537=DIRECTION('ref_axis',(-1.,0.,0.));
#13538=DIRECTION('',(-0.173648177666931,2.12657684957577E-17,0.984807753012208));
#13539=DIRECTION('center_axis',(0.,0.,-1.));
#13540=DIRECTION('ref_axis',(-1.,0.,0.));
#13541=DIRECTION('center_axis',(0.,0.,1.));
#13542=DIRECTION('ref_axis',(1.,0.,0.));
#13543=DIRECTION('center_axis',(0.,0.,-1.));
#13544=DIRECTION('ref_axis',(-1.,0.,0.));
#13545=DIRECTION('',(-0.087155742747658,-1.06735001383229E-17,0.996194698091746));
#13546=DIRECTION('center_axis',(0.,0.,-1.));
#13547=DIRECTION('ref_axis',(-1.,0.,0.));
#13548=DIRECTION('center_axis',(0.,0.,-1.));
#13549=DIRECTION('ref_axis',(-1.,0.,0.));
#13550=DIRECTION('center_axis',(0.,0.,-1.));
#13551=DIRECTION('ref_axis',(-1.,0.,0.));
#13552=DIRECTION('',(0.,0.,1.));
#13553=DIRECTION('center_axis',(0.,0.,-1.));
#13554=DIRECTION('ref_axis',(-1.,0.,0.));
#13555=DIRECTION('center_axis',(0.,0.,-1.));
#13556=DIRECTION('ref_axis',(-1.,0.,0.));
#13557=DIRECTION('center_axis',(0.,0.,-1.));
#13558=DIRECTION('ref_axis',(-1.,0.,0.));
#13559=DIRECTION('center_axis',(-1.22464679914735E-16,-1.,0.));
#13560=DIRECTION('ref_axis',(1.,-1.22464679914735E-16,0.));
#13561=DIRECTION('center_axis',(0.,0.,-1.));
#13562=DIRECTION('ref_axis',(-1.,0.,0.));
#13563=DIRECTION('center_axis',(0.,0.,-1.));
#13564=DIRECTION('ref_axis',(-1.,0.,0.));
#13565=DIRECTION('center_axis',(0.,0.,-1.));
#13566=DIRECTION('ref_axis',(-1.,0.,0.));
#13567=DIRECTION('',(0.,0.,1.));
#13568=DIRECTION('center_axis',(0.,0.,-1.));
#13569=DIRECTION('ref_axis',(-1.,0.,0.));
#13570=DIRECTION('center_axis',(0.,0.,-1.));
#13571=DIRECTION('ref_axis',(-1.,0.,0.));
#13572=DIRECTION('center_axis',(-1.22464679914735E-16,-1.,0.));
#13573=DIRECTION('ref_axis',(1.,-1.22464679914735E-16,0.));
#13574=DIRECTION('center_axis',(0.,0.,-1.));
#13575=DIRECTION('ref_axis',(-1.,0.,0.));
#13576=DIRECTION('center_axis',(0.,0.,-1.));
#13577=DIRECTION('ref_axis',(-1.,0.,0.));
#13578=DIRECTION('',(0.,0.,1.));
#13579=DIRECTION('center_axis',(0.,0.,-1.));
#13580=DIRECTION('ref_axis',(-1.,0.,0.));
#13581=DIRECTION('center_axis',(0.,0.,-1.));
#13582=DIRECTION('ref_axis',(-1.,0.,0.));
#13583=DIRECTION('center_axis',(0.,0.,-1.));
#13584=DIRECTION('ref_axis',(-1.,0.,0.));
#13585=DIRECTION('',(0.0871557427476568,-1.06735001383228E-17,-0.996194698091746));
#13586=DIRECTION('center_axis',(0.,0.,-1.));
#13587=DIRECTION('ref_axis',(-1.,0.,0.));
#13588=DIRECTION('center_axis',(0.,0.,1.));
#13589=DIRECTION('ref_axis',(1.,0.,0.));
#13590=DIRECTION('center_axis',(0.,0.,-1.));
#13591=DIRECTION('ref_axis',(-1.,0.,0.));
#13592=DIRECTION('',(0.173648177666931,2.12657684957577E-17,-0.984807753012208));
#13593=DIRECTION('center_axis',(0.,0.,-1.));
#13594=DIRECTION('ref_axis',(-1.,0.,0.));
#13595=DIRECTION('center_axis',(0.,0.,-1.));
#13596=DIRECTION('ref_axis',(-1.,0.,0.));
#13597=DIRECTION('center_axis',(0.,0.,-1.));
#13598=DIRECTION('ref_axis',(-1.,0.,0.));
#13599=DIRECTION('',(0.,0.,-1.));
#13600=DIRECTION('center_axis',(0.,0.,-1.));
#13601=DIRECTION('ref_axis',(-1.,0.,0.));
#13602=DIRECTION('center_axis',(0.,0.,1.));
#13603=DIRECTION('ref_axis',(1.,0.,0.));
#13604=DIRECTION('center_axis',(0.,0.,1.));
#13605=DIRECTION('ref_axis',(1.,0.,0.));
#13606=DIRECTION('center_axis',(0.,0.,1.));
#13607=DIRECTION('ref_axis',(1.,0.,0.));
#13608=DIRECTION('center_axis',(0.,0.,1.));
#13609=DIRECTION('ref_axis',(1.,0.,0.));
#13610=DIRECTION('center_axis',(0.,0.,-1.));
#13611=DIRECTION('ref_axis',(0.,-1.,0.));
#13612=DIRECTION('center_axis',(0.,0.,-1.));
#13613=DIRECTION('ref_axis',(0.,-1.,0.));
#13614=DIRECTION('center_axis',(0.,0.,-1.));
#13615=DIRECTION('ref_axis',(0.,-1.,0.));
#13616=DIRECTION('center_axis',(0.,0.,-1.));
#13617=DIRECTION('ref_axis',(0.,-1.,0.));
#13618=DIRECTION('axis',(0.,0.,1.));
#13619=DIRECTION('refdir',(1.,0.,0.));
#13620=DIRECTION('center_axis',(0.,0.,-1.));
#13621=DIRECTION('ref_axis',(-1.,0.,0.));
#13622=DIRECTION('center_axis',(0.,0.,-1.));
#13623=DIRECTION('ref_axis',(-1.,0.,0.));
#13624=DIRECTION('',(0.,0.,-1.));
#13625=DIRECTION('center_axis',(0.,0.,-1.));
#13626=DIRECTION('ref_axis',(-1.,0.,0.));
#13627=DIRECTION('center_axis',(0.,0.,-1.));
#13628=DIRECTION('ref_axis',(-1.,0.,0.));
#13629=DIRECTION('center_axis',(0.,0.,-1.));
#13630=DIRECTION('ref_axis',(-1.,0.,0.));
#13631=DIRECTION('center_axis',(1.22464679914735E-16,1.,0.));
#13632=DIRECTION('ref_axis',(1.,-1.22464679914735E-16,0.));
#13633=DIRECTION('center_axis',(0.,0.,-1.));
#13634=DIRECTION('ref_axis',(-1.,0.,0.));
#13635=DIRECTION('center_axis',(0.,0.,-1.));
#13636=DIRECTION('ref_axis',(-1.,0.,0.));
#13637=DIRECTION('',(0.,0.,-1.));
#13638=DIRECTION('center_axis',(0.,0.,-1.));
#13639=DIRECTION('ref_axis',(-1.,0.,0.));
#13640=DIRECTION('center_axis',(0.,0.,-1.));
#13641=DIRECTION('ref_axis',(-1.,0.,0.));
#13642=DIRECTION('center_axis',(1.22464679914735E-16,1.,0.));
#13643=DIRECTION('ref_axis',(1.,-1.22464679914735E-16,0.));
#13644=DIRECTION('center_axis',(0.,0.,-1.));
#13645=DIRECTION('ref_axis',(-1.,0.,0.));
#13646=DIRECTION('center_axis',(0.,0.,-1.));
#13647=DIRECTION('ref_axis',(-1.,0.,0.));
#13648=DIRECTION('center_axis',(0.,0.,-1.));
#13649=DIRECTION('ref_axis',(-1.,0.,0.));
#13650=DIRECTION('',(0.,0.,-1.));
#13651=DIRECTION('center_axis',(0.,0.,-1.));
#13652=DIRECTION('ref_axis',(-1.,0.,0.));
#13653=DIRECTION('center_axis',(0.,0.,-1.));
#13654=DIRECTION('ref_axis',(-1.,0.,0.));
#13655=DIRECTION('center_axis',(0.,0.,-1.));
#13656=DIRECTION('ref_axis',(-1.,0.,0.));
#13657=DIRECTION('center_axis',(1.22464679914735E-16,1.,0.));
#13658=DIRECTION('ref_axis',(1.,-1.22464679914735E-16,0.));
#13659=DIRECTION('center_axis',(0.,0.,-1.));
#13660=DIRECTION('ref_axis',(-1.,0.,0.));
#13661=DIRECTION('center_axis',(0.,0.,-1.));
#13662=DIRECTION('ref_axis',(-1.,0.,0.));
#13663=DIRECTION('center_axis',(0.,0.,1.));
#13664=DIRECTION('ref_axis',(1.,0.,0.));
#13665=DIRECTION('center_axis',(0.,0.,-1.));
#13666=DIRECTION('ref_axis',(-1.,0.,0.));
#13667=DIRECTION('',(0.996194698091745,1.21998664834562E-16,-0.0871557427476583));
#13668=DIRECTION('center_axis',(0.,0.,-1.));
#13669=DIRECTION('ref_axis',(-1.,0.,0.));
#13670=DIRECTION('center_axis',(0.,0.,-1.));
#13671=DIRECTION('ref_axis',(-1.,0.,0.));
#13672=DIRECTION('center_axis',(-1.22464679914735E-16,-1.,0.));
#13673=DIRECTION('ref_axis',(1.,-1.22464679914735E-16,0.));
#13674=DIRECTION('center_axis',(0.,0.,-1.));
#13675=DIRECTION('ref_axis',(-1.,0.,0.));
#13676=DIRECTION('center_axis',(0.,0.,-1.));
#13677=DIRECTION('ref_axis',(-1.,0.,0.));
#13678=DIRECTION('center_axis',(0.,0.,1.));
#13679=DIRECTION('ref_axis',(1.,0.,0.));
#13680=DIRECTION('center_axis',(0.,0.,-1.));
#13681=DIRECTION('ref_axis',(-1.,0.,0.));
#13682=DIRECTION('',(0.0523359562429446,6.4093061293238E-18,-0.998629534754574));
#13683=DIRECTION('center_axis',(0.,0.,-1.));
#13684=DIRECTION('ref_axis',(-1.,0.,0.));
#13685=DIRECTION('center_axis',(0.,0.,-1.));
#13686=DIRECTION('ref_axis',(-1.,0.,0.));
#13687=DIRECTION('',(-0.0523359562429425,6.40930612932355E-18,0.998629534754574));
#13688=DIRECTION('center_axis',(0.,0.,-1.));
#13689=DIRECTION('ref_axis',(-1.,0.,0.));
#13690=DIRECTION('center_axis',(0.,0.,-1.));
#13691=DIRECTION('ref_axis',(-1.,0.,0.));
#13692=DIRECTION('center_axis',(-1.22464679914735E-16,-1.,0.));
#13693=DIRECTION('ref_axis',(1.,-1.22464679914735E-16,0.));
#13694=DIRECTION('center_axis',(0.,0.,-1.));
#13695=DIRECTION('ref_axis',(-1.,0.,0.));
#13696=DIRECTION('center_axis',(0.,0.,-1.));
#13697=DIRECTION('ref_axis',(-1.,0.,0.));
#13698=DIRECTION('',(-0.996194698091746,1.21998664834562E-16,0.0871557427476584));
#13699=DIRECTION('center_axis',(0.,0.,-1.));
#13700=DIRECTION('ref_axis',(-1.,0.,0.));
#13701=DIRECTION('center_axis',(0.,0.,-1.));
#13702=DIRECTION('ref_axis',(-1.,0.,0.));
#13703=DIRECTION('center_axis',(1.22464679914735E-16,1.,0.));
#13704=DIRECTION('ref_axis',(1.,-1.22464679914735E-16,0.));
#13705=DIRECTION('center_axis',(0.,0.,-1.));
#13706=DIRECTION('ref_axis',(-1.,0.,0.));
#13707=DIRECTION('center_axis',(0.,0.,-1.));
#13708=DIRECTION('ref_axis',(0.,-1.,0.));
#13709=DIRECTION('center_axis',(0.,0.,1.));
#13710=DIRECTION('ref_axis',(1.,0.,0.));
#13711=DIRECTION('center_axis',(0.,0.,-1.));
#13712=DIRECTION('ref_axis',(0.,-1.,0.));
#13713=DIRECTION('center_axis',(0.,0.,1.));
#13714=DIRECTION('ref_axis',(1.,0.,0.));
#13715=DIRECTION('axis',(0.,0.,1.));
#13716=DIRECTION('refdir',(1.,0.,0.));
#13717=DIRECTION('center_axis',(0.,0.,-1.));
#13718=DIRECTION('ref_axis',(-1.,0.,0.));
#13719=DIRECTION('center_axis',(0.,0.,-1.));
#13720=DIRECTION('ref_axis',(-1.,0.,0.));
#13721=DIRECTION('',(0.,0.,-1.));
#13722=DIRECTION('center_axis',(0.,0.,-1.));
#13723=DIRECTION('ref_axis',(-1.,0.,0.));
#13724=DIRECTION('center_axis',(0.,0.,-1.));
#13725=DIRECTION('ref_axis',(-1.,0.,0.));
#13726=DIRECTION('center_axis',(0.,0.,-1.));
#13727=DIRECTION('ref_axis',(-1.,0.,0.));
#13728=DIRECTION('',(0.,0.,1.));
#13729=DIRECTION('center_axis',(0.,0.,-1.));
#13730=DIRECTION('ref_axis',(-1.,0.,0.));
#13731=DIRECTION('center_axis',(0.,0.,-1.));
#13732=DIRECTION('ref_axis',(0.,-1.,0.));
#13733=DIRECTION('center_axis',(0.,0.,1.));
#13734=DIRECTION('ref_axis',(1.,0.,0.));
#13735=DIRECTION('axis',(0.,0.,1.));
#13736=DIRECTION('refdir',(1.,0.,0.));
#13737=DIRECTION('center_axis',(0.,0.,1.));
#13738=DIRECTION('ref_axis',(1.,0.,0.));
#13739=DIRECTION('center_axis',(0.,0.,-1.));
#13740=DIRECTION('ref_axis',(-1.,0.,0.));
#13741=DIRECTION('',(-0.707106781186547,-8.65956056235493E-17,0.707106781186548));
#13742=DIRECTION('center_axis',(0.,0.,-1.));
#13743=DIRECTION('ref_axis',(-1.,0.,0.));
#13744=DIRECTION('center_axis',(0.,0.,-1.));
#13745=DIRECTION('ref_axis',(-1.,0.,0.));
#13746=DIRECTION('center_axis',(0.,0.,-1.));
#13747=DIRECTION('ref_axis',(-1.,0.,0.));
#13748=DIRECTION('',(0.,0.,-1.));
#13749=DIRECTION('center_axis',(0.,0.,-1.));
#13750=DIRECTION('ref_axis',(-1.,0.,0.));
#13751=DIRECTION('center_axis',(0.,0.,-1.));
#13752=DIRECTION('ref_axis',(-1.,0.,0.));
#13753=DIRECTION('',(0.707106781186545,-8.6595605623549E-17,-0.707106781186551));
#13754=DIRECTION('center_axis',(0.,0.,-1.));
#13755=DIRECTION('ref_axis',(-1.,0.,0.));
#13756=DIRECTION('center_axis',(0.,0.,-1.));
#13757=DIRECTION('ref_axis',(-1.,0.,0.));
#13758=DIRECTION('center_axis',(0.,0.,-1.));
#13759=DIRECTION('ref_axis',(-1.,0.,0.));
#13760=DIRECTION('',(0.,0.,1.));
#13761=DIRECTION('center_axis',(0.,0.,-1.));
#13762=DIRECTION('ref_axis',(-1.,0.,0.));
#13763=DIRECTION('center_axis',(0.,0.,-1.));
#13764=DIRECTION('ref_axis',(0.,-1.,0.));
#13765=DIRECTION('center_axis',(0.,0.,1.));
#13766=DIRECTION('ref_axis',(1.,0.,0.));
#13767=DIRECTION('',(0.,0.,1.));
#13768=DIRECTION('',(1.,0.,0.));
#13769=DIRECTION('',(-1.,0.,0.));
#13770=DIRECTION('',(0.,0.,-1.));
#13771=DIRECTION('',(0.,0.,-1.));
#13772=DIRECTION('',(1.,0.,0.));
#13773=DIRECTION('',(-1.,0.,0.));
#13774=DIRECTION('',(0.,0.,1.));
#13775=DIRECTION('',(-1.,0.,0.));
#13776=DIRECTION('',(0.,-1.,0.));
#13777=DIRECTION('',(0.,0.,1.));
#13778=DIRECTION('',(1.,0.,0.));
#13779=DIRECTION('',(0.,0.,-1.));
#13780=DIRECTION('',(1.,0.,0.));
#13781=DIRECTION('',(0.,0.,-1.));
#13782=DIRECTION('',(1.,0.,0.));
#13783=DIRECTION('',(0.,0.,1.));
#13784=DIRECTION('',(1.,0.,0.));
#13785=DIRECTION('',(0.,0.,-1.));
#13786=DIRECTION('',(1.,0.,0.));
#13787=DIRECTION('',(0.,0.,1.));
#13788=DIRECTION('',(1.,0.,0.));
#13789=DIRECTION('',(0.,0.,1.));
#13790=DIRECTION('',(1.,0.,0.));
#13791=DIRECTION('',(1.,0.,-3.14233320495882E-14));
#13792=DIRECTION('',(-3.14233320495882E-14,0.,-1.));
#13793=DIRECTION('',(-5.55111512312578E-17,1.05915854396386E-16,-1.));
#13794=DIRECTION('',(-1.,3.12250225675825E-17,5.55111512312578E-17));
#13795=DIRECTION('',(0.,0.,1.));
#13796=DIRECTION('',(1.,0.,0.));
#13797=DIRECTION('',(-1.,-1.03632557081398E-17,-1.23165366794353E-16));
#13798=DIRECTION('',(1.23165366794353E-16,6.87633951145162E-17,-1.));
#13799=DIRECTION('',(-1.03632557081401E-17,1.,6.87633951144766E-17));
#13800=DIRECTION('',(1.,1.03632557081401E-17,1.2490009027033E-16));
#13801=DIRECTION('',(-1.,0.,1.04744440165294E-14));
#13802=DIRECTION('',(1.04744440165294E-14,0.,1.));
#13803=DIRECTION('',(-1.,0.,1.04744440165294E-14));
#13804=DIRECTION('',(1.04744440165294E-14,0.,1.));
#13805=DIRECTION('',(-1.,0.,1.04744440165294E-14));
#13806=DIRECTION('',(1.04744440165294E-14,0.,1.));
#13807=DIRECTION('',(-1.,0.,1.04744440165294E-14));
#13808=DIRECTION('',(1.04744440165294E-14,0.,1.));
#13809=CARTESIAN_POINT('',(0.,0.,0.));
#13810=CARTESIAN_POINT('',(0.,0.,0.));
#13811=CARTESIAN_POINT('Origin',(-4.44089209850063E-13,37.83598559535,138.));
#13812=CARTESIAN_POINT('',(682.31,31.8359855953526,138.));
#13813=CARTESIAN_POINT('Origin',(682.31,37.8359855953526,138.));
#13814=CARTESIAN_POINT('',(685.31,31.8359855953526,138.));
#13815=CARTESIAN_POINT('',(-4.20716093542164E-13,31.83598559535,138.));
#13816=CARTESIAN_POINT('Origin',(685.31,37.8359855953527,138.));
#13817=CARTESIAN_POINT('Origin',(-4.44089209850063E-13,35.9826602645986,
63.0000000000002));
#13818=CARTESIAN_POINT('',(682.31,29.9826602646013,63.0000000000002));
#13819=CARTESIAN_POINT('Origin',(682.31,35.9826602646013,63.0000000000002));
#13820=CARTESIAN_POINT('',(685.31,29.9826602646013,63.0000000000002));
#13821=CARTESIAN_POINT('',(-4.20716093542165E-13,29.9826602645986,63.0000000000002));
#13822=CARTESIAN_POINT('Origin',(685.31,35.9826602646013,63.0000000000002));
#13823=CARTESIAN_POINT('Origin',(-4.44089209850063E-13,37.83598559535,138.));
#13824=CARTESIAN_POINT('',(-4.20716093542164E-13,31.83598559535,138.));
#13825=CARTESIAN_POINT('Origin',(-4.44089209850063E-13,37.83598559535,138.));
#13826=CARTESIAN_POINT('',(2.99999999999997,31.83598559535,138.));
#13827=CARTESIAN_POINT('',(-4.20716093542164E-13,31.83598559535,138.));
#13828=CARTESIAN_POINT('Origin',(2.9999999999999,37.83598559535,138.));
#13829=CARTESIAN_POINT('Origin',(-4.44089209850063E-13,35.9826602645986,
63.0000000000002));
#13830=CARTESIAN_POINT('',(-4.20716093542165E-13,29.9826602645986,63.0000000000002));
#13831=CARTESIAN_POINT('Origin',(-4.44089209850063E-13,35.9826602645986,
63.0000000000002));
#13832=CARTESIAN_POINT('',(2.99999999999996,29.9826602645986,63.0000000000002));
#13833=CARTESIAN_POINT('',(-4.20716093542165E-13,29.9826602645986,63.0000000000002));
#13834=CARTESIAN_POINT('Origin',(2.9999999999999,35.9826602645987,63.0000000000002));
#13835=CARTESIAN_POINT('Origin',(380.64910337319,10.,25.0462333534358));
#13836=CARTESIAN_POINT('',(380.64910337319,3.,31.3962333534358));
#13837=CARTESIAN_POINT('Origin',(380.64910337319,3.,25.0462333534358));
#13838=CARTESIAN_POINT('',(380.64910337319,-4.44089209850063E-15,31.3962333534358));
#13839=CARTESIAN_POINT('',(380.64910337319,10.,31.3962333534358));
#13840=CARTESIAN_POINT('Origin',(380.64910337319,-3.06727895069828E-15,
25.0462333534358));
#13841=CARTESIAN_POINT('Origin',(304.66089662681,10.,25.0462333534316));
#13842=CARTESIAN_POINT('',(304.66089662681,3.,31.3962333534329));
#13843=CARTESIAN_POINT('Origin',(304.66089662681,3.,25.0462333534316));
#13844=CARTESIAN_POINT('',(304.66089662681,-4.44089209850063E-15,31.3962333534329));
#13845=CARTESIAN_POINT('',(304.66089662681,10.,31.3962333534329));
#13846=CARTESIAN_POINT('Origin',(304.66089662681,-3.06727895069777E-15,
25.0462333534316));
#13847=CARTESIAN_POINT('Origin',(342.655,9.99999999999997,213.158883372056));
#13848=CARTESIAN_POINT('',(342.655,3.,219.508883372057));
#13849=CARTESIAN_POINT('Origin',(342.655,3.,213.158883372056));
#13850=CARTESIAN_POINT('',(342.655,-2.77555756156289E-14,219.508883372057));
#13851=CARTESIAN_POINT('',(342.655,9.99999999999997,219.508883372057));
#13852=CARTESIAN_POINT('Origin',(342.655,-2.61044344231412E-14,213.158883372056));
#13853=CARTESIAN_POINT('Origin',(39.5,4.5,32.0000000000144));
#13854=CARTESIAN_POINT('',(39.5,3.,38.4629015223999));
#13855=CARTESIAN_POINT('Origin',(39.5,3.,32.0000000000144));
#13856=CARTESIAN_POINT('',(39.5,-5.55111512312578E-16,38.4629015223999));
#13857=CARTESIAN_POINT('',(39.5,4.5,38.4629015223999));
#13858=CARTESIAN_POINT('Origin',(39.5,0.,32.0000000000144));
#13859=CARTESIAN_POINT('Origin',(645.81,4.5,32.0000000000145));
#13860=CARTESIAN_POINT('',(645.81,3.,38.4629015224));
#13861=CARTESIAN_POINT('Origin',(645.81,3.,32.0000000000145));
#13862=CARTESIAN_POINT('',(645.81,0.,38.4629015224));
#13863=CARTESIAN_POINT('',(645.81,4.5,38.4629015224));
#13864=CARTESIAN_POINT('Origin',(645.81,0.,32.0000000000145));
#13865=CARTESIAN_POINT('Origin',(39.7099999999999,4.5,216.5));
#13866=CARTESIAN_POINT('',(39.7099999999999,3.,222.85));
#13867=CARTESIAN_POINT('Origin',(39.7099999999999,3.,216.5));
#13868=CARTESIAN_POINT('',(39.7099999999999,0.,222.85));
#13869=CARTESIAN_POINT('',(39.7099999999999,4.5,222.85));
#13870=CARTESIAN_POINT('Origin',(39.7099999999999,0.,216.5));
#13871=CARTESIAN_POINT('Origin',(645.6,4.5,216.5));
#13872=CARTESIAN_POINT('',(645.6,3.,222.85));
#13873=CARTESIAN_POINT('Origin',(645.6,3.,216.5));
#13874=CARTESIAN_POINT('',(645.6,0.,222.85));
#13875=CARTESIAN_POINT('',(645.6,4.5,222.85));
#13876=CARTESIAN_POINT('Origin',(645.6,0.,216.5));
#13877=CARTESIAN_POINT('Origin',(0.,66.,4.));
#13878=CARTESIAN_POINT('',(0.,66.,4.));
#13879=CARTESIAN_POINT('',(0.127016653792582,66.,4.));
#13880=CARTESIAN_POINT('',(0.,66.,4.));
#13881=CARTESIAN_POINT('',(4.,69.,4.));
#13882=CARTESIAN_POINT('Origin',(4.,65.,4.));
#13883=CARTESIAN_POINT('',(0.,69.,4.));
#13884=CARTESIAN_POINT('',(685.31,69.,3.99999999999926));
#13885=CARTESIAN_POINT('',(0.,69.,4.));
#13886=CARTESIAN_POINT('Origin',(4.,66.,175.030507120983));
#13887=CARTESIAN_POINT('',(4.,69.,175.030507120983));
#13888=CARTESIAN_POINT('',(0.,69.,175.030507120983));
#13889=CARTESIAN_POINT('',(685.31,69.,175.030507120983));
#13890=CARTESIAN_POINT('',(0.127016653792575,66.,175.030507120983));
#13891=CARTESIAN_POINT('Origin',(4.,65.,175.030507120983));
#13892=CARTESIAN_POINT('',(0.,66.,175.030507120983));
#13893=CARTESIAN_POINT('',(4.,66.,175.030507120983));
#13894=CARTESIAN_POINT('',(0.,66.,175.030507120983));
#13895=CARTESIAN_POINT('Origin',(685.31,69.,0.));
#13896=CARTESIAN_POINT('',(681.31,68.9999999999999,4.));
#13897=CARTESIAN_POINT('',(685.31,69.,4.));
#13898=CARTESIAN_POINT('',(4.,69.,3.99999999999999));
#13899=CARTESIAN_POINT('',(681.31,68.9999999999999,175.030507120983));
#13900=CARTESIAN_POINT('',(685.31,69.,175.030507120983));
#13901=CARTESIAN_POINT('',(681.31,68.9999999999999,175.030507120983));
#13902=CARTESIAN_POINT('Origin',(685.31,66.,-4.73106402539129E-16));
#13903=CARTESIAN_POINT('',(4.,66.,4.));
#13904=CARTESIAN_POINT('',(4.,66.,175.030507120983));
#13905=CARTESIAN_POINT('',(4.,66.,3.99999999999999));
#13906=CARTESIAN_POINT('',(681.31,66.,4.));
#13907=CARTESIAN_POINT('',(685.31,66.,4.));
#13908=CARTESIAN_POINT('',(681.31,65.9999999999999,175.030507120983));
#13909=CARTESIAN_POINT('',(681.31,65.9999999999999,175.030507120983));
#13910=CARTESIAN_POINT('',(685.31,66.,175.030507120983));
#13911=CARTESIAN_POINT('Origin',(685.31,66.,175.030507120983));
#13912=CARTESIAN_POINT('',(685.31,66.,175.030507120983));
#13913=CARTESIAN_POINT('',(685.182983346207,66.,175.030507120983));
#13914=CARTESIAN_POINT('',(685.31,66.,175.030507120983));
#13915=CARTESIAN_POINT('Origin',(681.31,64.9999999999999,175.030507120983));
#13916=CARTESIAN_POINT('',(685.31,69.,175.030507120983));
#13917=CARTESIAN_POINT('',(685.31,69.,175.030507120983));
#13918=CARTESIAN_POINT('',(685.31,69.,175.030507120983));
#13919=CARTESIAN_POINT('Origin',(681.31,65.9999999999999,4.));
#13920=CARTESIAN_POINT('',(685.31,69.,4.));
#13921=CARTESIAN_POINT('',(685.31,69.,4.));
#13922=CARTESIAN_POINT('',(685.182983346207,66.,4.));
#13923=CARTESIAN_POINT('Origin',(681.31,64.9999999999999,4.));
#13924=CARTESIAN_POINT('',(685.31,66.,4.));
#13925=CARTESIAN_POINT('',(685.31,66.,4.));
#13926=CARTESIAN_POINT('',(685.31,66.,4.));
#13927=CARTESIAN_POINT('Origin',(685.31,4.00000000000003,236.));
#13928=CARTESIAN_POINT('',(685.31,4.00000000000003,236.));
#13929=CARTESIAN_POINT('',(685.31,4.00000000000003,233.));
#13930=CARTESIAN_POINT('',(685.31,4.00000000000003,236.));
#13931=CARTESIAN_POINT('',(685.31,0.,232.));
#13932=CARTESIAN_POINT('Origin',(685.31,4.,232.));
#13933=CARTESIAN_POINT('',(685.31,3.,232.));
#13934=CARTESIAN_POINT('',(685.31,3.,232.));
#13935=CARTESIAN_POINT('Origin',(685.31,4.,232.));
#13936=CARTESIAN_POINT('Origin',(685.31,3.,232.));
#13937=CARTESIAN_POINT('',(685.31,35.6607111673065,236.));
#13938=CARTESIAN_POINT('',(685.31,38.1,236.));
#13939=CARTESIAN_POINT('',(685.31,35.6607111673065,233.));
#13940=CARTESIAN_POINT('',(685.31,38.1,233.));
#13941=CARTESIAN_POINT('',(685.31,35.6607111673065,233.));
#13942=CARTESIAN_POINT('Origin',(0.,0.,232.));
#13943=CARTESIAN_POINT('',(0.,0.,232.));
#13944=CARTESIAN_POINT('',(0.,3.,232.));
#13945=CARTESIAN_POINT('',(0.,0.,232.));
#13946=CARTESIAN_POINT('',(0.,4.00000000000003,236.));
#13947=CARTESIAN_POINT('Origin',(0.,4.,232.));
#13948=CARTESIAN_POINT('',(0.,4.00000000000003,233.));
#13949=CARTESIAN_POINT('',(0.,4.00000000000003,233.));
#13950=CARTESIAN_POINT('Origin',(0.,4.,232.));
#13951=CARTESIAN_POINT('Origin',(0.,4.00000000000003,233.));
#13952=CARTESIAN_POINT('',(0.,0.,201.));
#13953=CARTESIAN_POINT('',(0.,0.,236.));
#13954=CARTESIAN_POINT('',(0.,3.,201.));
#13955=CARTESIAN_POINT('',(0.,3.,236.));
#13956=CARTESIAN_POINT('',(0.,3.,201.));
#13957=CARTESIAN_POINT('Origin',(685.31,39.2168287216494,233.831400540487));
#13958=CARTESIAN_POINT('',(685.31,39.2168287216494,233.831400540487));
#13959=CARTESIAN_POINT('',(685.31,36.5497405558922,232.457850135122));
#13960=CARTESIAN_POINT('',(685.31,39.2168287216494,233.831400540487));
#13961=CARTESIAN_POINT('Origin',(685.31,35.6607111673065,232.));
#13962=CARTESIAN_POINT('Origin',(685.31,35.6607111673065,232.));
#13963=CARTESIAN_POINT('Origin',(685.31,35.6607111673065,233.));
#13964=CARTESIAN_POINT('',(685.31,68.5561175543429,176.86190766147));
#13965=CARTESIAN_POINT('',(685.31,69.,176.));
#13966=CARTESIAN_POINT('',(685.31,65.8890293885857,175.488357256105));
#13967=CARTESIAN_POINT('',(685.31,66.3329118342428,174.626449594635));
#13968=CARTESIAN_POINT('',(685.31,65.8890293885857,175.488357256105));
#13969=CARTESIAN_POINT('Origin',(0.,35.6607111673065,236.));
#13970=CARTESIAN_POINT('',(0.,35.6607111673065,236.));
#13971=CARTESIAN_POINT('',(0.,35.6607111673065,233.));
#13972=CARTESIAN_POINT('',(0.,35.6607111673065,236.));
#13973=CARTESIAN_POINT('',(0.,39.2168287216494,233.831400540487));
#13974=CARTESIAN_POINT('Origin',(0.,35.6607111673065,232.));
#13975=CARTESIAN_POINT('',(0.,36.5497405558922,232.457850135122));
#13976=CARTESIAN_POINT('',(0.,36.5497405558922,232.457850135122));
#13977=CARTESIAN_POINT('Origin',(0.,35.6607111673065,232.));
#13978=CARTESIAN_POINT('Origin',(0.,36.5497405558922,232.457850135122));
#13979=CARTESIAN_POINT('',(0.,38.1,236.));
#13980=CARTESIAN_POINT('',(0.,38.1,233.));
#13981=CARTESIAN_POINT('Origin',(685.31,69.,175.030507120983));
#13982=CARTESIAN_POINT('Origin',(685.31,65.,175.030507120983));
#13983=CARTESIAN_POINT('Origin',(685.31,65.,175.030507120983));
#13984=CARTESIAN_POINT('Origin',(0.,68.5561175543429,176.86190766147));
#13985=CARTESIAN_POINT('',(0.,68.5561175543429,176.86190766147));
#13986=CARTESIAN_POINT('',(0.,65.8890293885857,175.488357256105));
#13987=CARTESIAN_POINT('',(0.,68.5561175543429,176.86190766147));
#13988=CARTESIAN_POINT('Origin',(0.,65.,175.030507120983));
#13989=CARTESIAN_POINT('Origin',(0.,65.,175.030507120983));
#13990=CARTESIAN_POINT('Origin',(0.,66.,175.030507120983));
#13991=CARTESIAN_POINT('',(0.,69.,176.));
#13992=CARTESIAN_POINT('',(0.,66.3329118342428,174.626449594635));
#13993=CARTESIAN_POINT('Origin',(685.31,65.,0.));
#13994=CARTESIAN_POINT('',(685.31,65.,0.));
#13995=CARTESIAN_POINT('',(685.31,65.,3.));
#13996=CARTESIAN_POINT('',(685.31,65.,0.));
#13997=CARTESIAN_POINT('Origin',(685.31,65.,4.));
#13998=CARTESIAN_POINT('Origin',(685.31,65.,4.));
#13999=CARTESIAN_POINT('Origin',(685.31,66.,4.));
#14000=CARTESIAN_POINT('',(685.31,4.,0.));
#14001=CARTESIAN_POINT('',(685.31,0.,0.));
#14002=CARTESIAN_POINT('',(685.31,4.,3.));
#14003=CARTESIAN_POINT('',(685.31,0.,3.));
#14004=CARTESIAN_POINT('',(685.31,4.,3.));
#14005=CARTESIAN_POINT('Origin',(0.,69.,4.));
#14006=CARTESIAN_POINT('',(0.,65.,0.));
#14007=CARTESIAN_POINT('Origin',(0.,65.,4.));
#14008=CARTESIAN_POINT('',(0.,65.,3.));
#14009=CARTESIAN_POINT('',(0.,65.,3.));
#14010=CARTESIAN_POINT('Origin',(0.,65.,4.));
#14011=CARTESIAN_POINT('Origin',(685.31,-4.89858719658941E-16,4.));
#14012=CARTESIAN_POINT('',(685.31,-4.89858719658941E-16,4.));
#14013=CARTESIAN_POINT('',(685.31,3.,4.));
#14014=CARTESIAN_POINT('',(685.31,-4.89858719658941E-16,4.));
#14015=CARTESIAN_POINT('Origin',(685.31,4.,4.));
#14016=CARTESIAN_POINT('Origin',(685.31,4.,4.));
#14017=CARTESIAN_POINT('Origin',(685.31,4.,3.));
#14018=CARTESIAN_POINT('',(685.31,-7.47034547479886E-15,61.));
#14019=CARTESIAN_POINT('',(685.31,0.,0.));
#14020=CARTESIAN_POINT('',(685.31,2.99999999999999,61.));
#14021=CARTESIAN_POINT('',(685.31,3.,3.67394039744206E-16));
#14022=CARTESIAN_POINT('',(685.31,-7.47034547479886E-15,61.));
#14023=CARTESIAN_POINT('Origin',(0.,4.,0.));
#14024=CARTESIAN_POINT('',(0.,4.,0.));
#14025=CARTESIAN_POINT('',(0.,4.,3.));
#14026=CARTESIAN_POINT('',(0.,4.,0.));
#14027=CARTESIAN_POINT('',(0.,-4.89858719658941E-16,4.));
#14028=CARTESIAN_POINT('Origin',(0.,4.,4.));
#14029=CARTESIAN_POINT('',(0.,3.,4.));
#14030=CARTESIAN_POINT('',(0.,3.,4.));
#14031=CARTESIAN_POINT('Origin',(0.,4.,4.));
#14032=CARTESIAN_POINT('Origin',(0.,3.,4.));
#14033=CARTESIAN_POINT('',(0.,0.,0.));
#14034=CARTESIAN_POINT('',(0.,0.,3.));
#14035=CARTESIAN_POINT('Origin',(685.31,3.,3.67394039744206E-16));
#14036=CARTESIAN_POINT('',(0.,2.99999999999999,61.));
#14037=CARTESIAN_POINT('',(0.,3.,3.67394039744206E-16));
#14038=CARTESIAN_POINT('',(685.31,2.99999999999999,61.));
#14039=CARTESIAN_POINT('',(685.31,3.,4.));
#14040=CARTESIAN_POINT('Origin',(685.31,-7.47034547479886E-15,61.));
#14041=CARTESIAN_POINT('',(0.,-7.47034547479886E-15,61.));
#14042=CARTESIAN_POINT('',(0.,-7.47034547479886E-15,61.));
#14043=CARTESIAN_POINT('',(685.31,-7.47034547479886E-15,61.));
#14044=CARTESIAN_POINT('Origin',(685.31,0.,0.));
#14045=CARTESIAN_POINT('',(0.,0.,0.));
#14046=CARTESIAN_POINT('',(685.31,-4.89858719658941E-16,4.));
#14047=CARTESIAN_POINT('Origin',(685.31,4.,4.));
#14048=CARTESIAN_POINT('',(685.31,4.,0.));
#14049=CARTESIAN_POINT('Origin',(685.31,0.,0.));
#14050=CARTESIAN_POINT('',(685.31,65.,0.));
#14051=CARTESIAN_POINT('Origin',(685.31,65.,4.));
#14052=CARTESIAN_POINT('Origin',(685.31,65.,175.030507120983));
#14053=CARTESIAN_POINT('',(685.31,68.5561175543429,176.86190766147));
#14054=CARTESIAN_POINT('Origin',(685.31,69.,176.));
#14055=CARTESIAN_POINT('',(685.31,39.2168287216494,233.831400540487));
#14056=CARTESIAN_POINT('Origin',(685.31,35.6607111673065,232.));
#14057=CARTESIAN_POINT('',(685.31,35.6607111673065,236.));
#14058=CARTESIAN_POINT('Origin',(685.31,38.1,236.));
#14059=CARTESIAN_POINT('',(685.31,4.00000000000003,236.));
#14060=CARTESIAN_POINT('Origin',(685.31,4.,232.));
#14061=CARTESIAN_POINT('',(685.31,0.,232.));
#14062=CARTESIAN_POINT('Origin',(685.31,0.,236.));
#14063=CARTESIAN_POINT('',(685.31,0.,201.));
#14064=CARTESIAN_POINT('',(685.31,0.,201.));
#14065=CARTESIAN_POINT('',(685.31,0.,236.));
#14066=CARTESIAN_POINT('Origin',(685.31,3.,201.));
#14067=CARTESIAN_POINT('',(685.31,3.,201.));
#14068=CARTESIAN_POINT('',(685.31,3.,201.));
#14069=CARTESIAN_POINT('',(685.31,3.,201.));
#14070=CARTESIAN_POINT('Origin',(685.31,3.,236.));
#14071=CARTESIAN_POINT('',(685.31,3.,232.));
#14072=CARTESIAN_POINT('',(685.31,3.,236.));
#14073=CARTESIAN_POINT('Origin',(685.31,4.,232.));
#14074=CARTESIAN_POINT('',(685.31,4.00000000000003,233.));
#14075=CARTESIAN_POINT('Origin',(685.31,38.1,233.));
#14076=CARTESIAN_POINT('',(685.31,35.6607111673065,233.));
#14077=CARTESIAN_POINT('Origin',(685.31,35.6607111673065,232.));
#14078=CARTESIAN_POINT('',(685.31,36.5497405558922,232.457850135122));
#14079=CARTESIAN_POINT('Origin',(685.31,66.3329118342428,174.626449594635));
#14080=CARTESIAN_POINT('',(685.31,65.8890293885857,175.488357256105));
#14081=CARTESIAN_POINT('Origin',(685.31,65.,175.030507120983));
#14082=CARTESIAN_POINT('',(4.,66.,175.030507120983));
#14083=CARTESIAN_POINT('',(685.31,66.,175.030507120983));
#14084=CARTESIAN_POINT('Origin',(685.31,65.,4.));
#14085=CARTESIAN_POINT('',(685.31,65.,3.));
#14086=CARTESIAN_POINT('',(685.31,66.,4.));
#14087=CARTESIAN_POINT('',(0.,66.,4.));
#14088=CARTESIAN_POINT('Origin',(685.31,0.,3.));
#14089=CARTESIAN_POINT('',(685.31,4.,3.));
#14090=CARTESIAN_POINT('Origin',(685.31,4.,4.));
#14091=CARTESIAN_POINT('Origin',(685.31,4.,4.));
#14092=CARTESIAN_POINT('Origin',(0.,4.,4.));
#14093=CARTESIAN_POINT('Origin',(681.31,64.9999999999999,4.));
#14094=CARTESIAN_POINT('',(685.31,64.9999999999999,4.));
#14095=CARTESIAN_POINT('Origin',(681.31,64.9999999999999,4.));
#14096=CARTESIAN_POINT('',(682.31,64.9999999999999,4.));
#14097=CARTESIAN_POINT('',(685.31,65.,4.));
#14098=CARTESIAN_POINT('Origin',(681.31,64.9999999999999,4.));
#14099=CARTESIAN_POINT('Origin',(681.31,64.9999999999999,175.030507120983));
#14100=CARTESIAN_POINT('',(685.31,65.,175.030507120983));
#14101=CARTESIAN_POINT('Origin',(681.31,64.9999999999999,175.030507120983));
#14102=CARTESIAN_POINT('',(682.31,64.9999999999999,175.030507120983));
#14103=CARTESIAN_POINT('Origin',(681.31,64.9999999999999,175.030507120983));
#14104=CARTESIAN_POINT('',(682.31,64.9999999999999,175.030507120983));
#14105=CARTESIAN_POINT('Origin',(681.31,64.9999999999999,175.030507120983));
#14106=CARTESIAN_POINT('',(685.31,65.,3.99999999999999));
#14107=CARTESIAN_POINT('Origin',(681.31,64.9999999999999,175.030507120983));
#14108=CARTESIAN_POINT('',(682.31,64.9999999999999,3.99999999999999));
#14109=CARTESIAN_POINT('Origin',(685.31,8.99999999999998,175.030507120983));
#14110=CARTESIAN_POINT('',(682.31,62.0111994331027,175.030507120983));
#14111=CARTESIAN_POINT('',(682.31,8.99999999999996,175.030507120983));
#14112=CARTESIAN_POINT('',(685.31,62.0111994331027,175.030507120983));
#14113=CARTESIAN_POINT('',(682.31,62.0111994331027,175.030507120983));
#14114=CARTESIAN_POINT('',(685.31,2.6801128335108E-12,175.030507120983));
#14115=CARTESIAN_POINT('Origin',(685.31,66.,4.));
#14116=CARTESIAN_POINT('',(685.31,9.00000000000001,3.99999999999999));
#14117=CARTESIAN_POINT('',(685.31,2.67932155613579E-12,3.99999999999999));
#14118=CARTESIAN_POINT('',(682.31,8.99999999999999,3.99999999999999));
#14119=CARTESIAN_POINT('',(685.31,9.00000000000001,3.99999999999999));
#14120=CARTESIAN_POINT('',(682.31,66.,4.));
#14121=CARTESIAN_POINT('Origin',(685.31,2.6801128335108E-12,4.3494038380127E-28));
#14122=CARTESIAN_POINT('',(685.31,34.9708140306692,228.641008611614));
#14123=CARTESIAN_POINT('',(685.31,62.0111994331027,175.030507120983));
#14124=CARTESIAN_POINT('',(685.31,8.99999999999998,228.641008611614));
#14125=CARTESIAN_POINT('',(685.31,34.9708140306692,228.641008611614));
#14126=CARTESIAN_POINT('',(685.31,9.00000000000001,1.46055919932435E-15));
#14127=CARTESIAN_POINT('Origin',(682.31,2.66963838949427E-12,4.33240545405031E-28));
#14128=CARTESIAN_POINT('',(682.31,8.99999999999997,228.641008611614));
#14129=CARTESIAN_POINT('',(682.31,8.99999999999999,3.99999999999999));
#14130=CARTESIAN_POINT('',(682.31,34.9708140306692,228.641008611614));
#14131=CARTESIAN_POINT('',(682.31,34.9708140306692,228.641008611614));
#14132=CARTESIAN_POINT('',(682.31,62.0111994331027,175.030507120983));
#14133=CARTESIAN_POINT('Origin',(685.31,9.00000000000001,3.99999999999999));
#14134=CARTESIAN_POINT('',(682.31,8.99999999999997,228.641008611614));
#14135=CARTESIAN_POINT('Origin',(682.31,34.9708140306692,228.641008611614));
#14136=CARTESIAN_POINT('',(682.31,34.9708140306692,228.641008611614));
#14137=CARTESIAN_POINT('Origin',(682.31,62.0111994331027,175.030507120983));
#14138=CARTESIAN_POINT('Origin',(4.,65.,175.030507120983));
#14139=CARTESIAN_POINT('',(3.,65.,175.030507120983));
#14140=CARTESIAN_POINT('Origin',(4.,65.,175.030507120983));
#14141=CARTESIAN_POINT('',(-1.73472347597681E-15,65.,175.030507120983));
#14142=CARTESIAN_POINT('Origin',(4.,65.,175.030507120983));
#14143=CARTESIAN_POINT('',(-3.4914813388431E-15,65.,175.030507120983));
#14144=CARTESIAN_POINT('Origin',(4.,65.,4.));
#14145=CARTESIAN_POINT('',(-3.43664881674456E-15,65.,4.));
#14146=CARTESIAN_POINT('Origin',(4.,65.,4.));
#14147=CARTESIAN_POINT('',(3.,65.,4.));
#14148=CARTESIAN_POINT('Origin',(4.,65.,4.));
#14149=CARTESIAN_POINT('',(3.,65.,4.));
#14150=CARTESIAN_POINT('Origin',(4.,65.,3.99999999999999));
#14151=CARTESIAN_POINT('',(-3.46944695195361E-15,65.,175.030507120983));
#14152=CARTESIAN_POINT('Origin',(4.,65.,3.99999999999999));
#14153=CARTESIAN_POINT('',(3.,65.,175.030507120983));
#14154=CARTESIAN_POINT('Origin',(0.,66.,175.030507120983));
#14155=CARTESIAN_POINT('',(-1.37735958159548E-14,62.0111994331051,175.030507120983));
#14156=CARTESIAN_POINT('',(-2.30284541435921E-13,1.04744440165302E-14,175.030507120983));
#14157=CARTESIAN_POINT('',(2.99999999999999,62.0111994331051,175.030507120983));
#14158=CARTESIAN_POINT('',(3.00000000000022,62.0111994331051,175.030507120983));
#14159=CARTESIAN_POINT('',(3.,66.,175.030507120983));
#14160=CARTESIAN_POINT('Origin',(-1.99059518868339E-13,9.00000000000001,
3.99999999999998));
#14161=CARTESIAN_POINT('',(2.9999999999998,8.99999999999999,3.99999999999998));
#14162=CARTESIAN_POINT('',(2.9999999999998,8.99999999999999,3.99999999999998));
#14163=CARTESIAN_POINT('',(-1.98861209386333E-13,9.00000000000001,3.99999999999998));
#14164=CARTESIAN_POINT('',(-1.99059518868339E-13,9.00000000000001,3.99999999999998));
#14165=CARTESIAN_POINT('',(-2.30284541435921E-13,8.95275675690144E-15,3.99999999999998));
#14166=CARTESIAN_POINT('Origin',(-2.30284541435921E-13,1.04744440165302E-14,
1.699838396239E-30));
#14167=CARTESIAN_POINT('',(3.14233320495966E-14,9.00000000000237,228.641008611614));
#14168=CARTESIAN_POINT('',(-1.98861209386333E-13,9.00000000000001,1.46055919932435E-15));
#14169=CARTESIAN_POINT('',(1.22099944592244E-13,34.9708140306716,228.641008611614));
#14170=CARTESIAN_POINT('',(3.14233320495966E-14,9.00000000000237,228.641008611614));
#14171=CARTESIAN_POINT('',(1.22099944592244E-13,34.9708140306716,228.641008611614));
#14172=CARTESIAN_POINT('Origin',(2.99999999999977,8.04569168006329E-28,
1.30568988869375E-43));
#14173=CARTESIAN_POINT('',(3.00000000000012,34.9708140306716,228.641008611614));
#14174=CARTESIAN_POINT('',(3.00000000000012,34.9708140306716,228.641008611614));
#14175=CARTESIAN_POINT('',(3.00000000000003,9.00000000000236,228.641008611614));
#14176=CARTESIAN_POINT('',(3.00000000000003,9.00000000000236,228.641008611614));
#14177=CARTESIAN_POINT('',(2.9999999999998,8.99999999999997,175.030507120983));
#14178=CARTESIAN_POINT('Origin',(-1.99059518868339E-13,8.99999999999998,
175.030507120983));
#14179=CARTESIAN_POINT('',(3.00000000000003,9.00000000000236,228.641008611614));
#14180=CARTESIAN_POINT('Origin',(3.00000000000012,34.9708140306716,228.641008611614));
#14181=CARTESIAN_POINT('',(3.00000000000012,34.9708140306716,228.641008611614));
#14182=CARTESIAN_POINT('Origin',(3.00000000000003,9.00000000000236,228.641008611614));
#14183=CARTESIAN_POINT('',(0.,0.,0.));
#14184=CARTESIAN_POINT('Origin',(63.9999999999783,34.4999999999999,-2.22044604925031E-13));
#14185=CARTESIAN_POINT('',(57.9999999999783,34.4999999999999,682.31));
#14186=CARTESIAN_POINT('Origin',(63.9999999999783,34.4999999999999,682.31));
#14187=CARTESIAN_POINT('',(57.9999999999783,34.4999999999999,685.31));
#14188=CARTESIAN_POINT('',(57.9999999999783,34.4999999999999,-2.22044604925031E-13));
#14189=CARTESIAN_POINT('Origin',(63.9999999999783,34.4999999999999,685.31));
#14190=CARTESIAN_POINT('Origin',(138.999999999978,34.5,-2.22044604925031E-13));
#14191=CARTESIAN_POINT('',(132.999999999978,34.5,682.31));
#14192=CARTESIAN_POINT('Origin',(138.999999999978,34.5,682.31));
#14193=CARTESIAN_POINT('',(132.999999999978,34.5,685.31));
#14194=CARTESIAN_POINT('',(132.999999999978,34.5,-2.22044604925031E-13));
#14195=CARTESIAN_POINT('Origin',(138.999999999978,34.5,685.31));
#14196=CARTESIAN_POINT('Origin',(63.9999999999783,34.4999999999999,-2.22044604925031E-13));
#14197=CARTESIAN_POINT('',(57.9999999999783,34.4999999999999,-2.22044604925031E-13));
#14198=CARTESIAN_POINT('Origin',(63.9999999999783,34.4999999999999,-2.22044604925031E-13));
#14199=CARTESIAN_POINT('',(57.9999999999783,34.4999999999999,2.99999999999991));
#14200=CARTESIAN_POINT('',(57.9999999999783,34.4999999999999,-2.22044604925031E-13));
#14201=CARTESIAN_POINT('Origin',(63.9999999999783,34.4999999999999,2.99999999999989));
#14202=CARTESIAN_POINT('Origin',(138.999999999978,34.5,-2.22044604925031E-13));
#14203=CARTESIAN_POINT('',(132.999999999978,34.5,-2.22044604925031E-13));
#14204=CARTESIAN_POINT('Origin',(138.999999999978,34.5,-2.22044604925031E-13));
#14205=CARTESIAN_POINT('',(132.999999999978,34.5,2.99999999999991));
#14206=CARTESIAN_POINT('',(132.999999999978,34.5,-2.22044604925031E-13));
#14207=CARTESIAN_POINT('Origin',(138.999999999978,34.5,2.99999999999989));
#14208=CARTESIAN_POINT('Origin',(175.50000000002,4.5,39.4999999999858));
#14209=CARTESIAN_POINT('',(175.50000000002,3.,45.8499999999858));
#14210=CARTESIAN_POINT('Origin',(175.50000000002,3.,39.4999999999858));
#14211=CARTESIAN_POINT('',(175.50000000002,0.,45.8499999999858));
#14212=CARTESIAN_POINT('',(175.50000000002,4.5,45.8499999999858));
#14213=CARTESIAN_POINT('Origin',(175.50000000002,0.,39.4999999999858));
#14214=CARTESIAN_POINT('Origin',(175.500000000001,4.5,645.809999999986));
#14215=CARTESIAN_POINT('',(175.500000000001,3.,652.159999999986));
#14216=CARTESIAN_POINT('Origin',(175.500000000001,3.,645.809999999986));
#14217=CARTESIAN_POINT('',(175.500000000001,0.,652.159999999986));
#14218=CARTESIAN_POINT('',(175.500000000001,4.5,652.159999999986));
#14219=CARTESIAN_POINT('Origin',(175.500000000001,0.,645.809999999986));
#14220=CARTESIAN_POINT('Origin',(32.0000000000012,4.5,39.5000000000189));
#14221=CARTESIAN_POINT('',(32.0000000000012,3.,45.8500000000188));
#14222=CARTESIAN_POINT('Origin',(32.0000000000012,3.,39.5000000000189));
#14223=CARTESIAN_POINT('',(32.0000000000012,0.,45.8500000000188));
#14224=CARTESIAN_POINT('',(32.0000000000012,4.5,45.8500000000188));
#14225=CARTESIAN_POINT('Origin',(32.0000000000012,0.,39.5000000000189));
#14226=CARTESIAN_POINT('Origin',(32.0000000000012,4.5,645.809999999981));
#14227=CARTESIAN_POINT('',(32.0000000000012,3.,652.159999999981));
#14228=CARTESIAN_POINT('Origin',(32.0000000000012,3.,645.809999999981));
#14229=CARTESIAN_POINT('',(32.0000000000012,0.,652.159999999981));
#14230=CARTESIAN_POINT('',(32.0000000000012,4.5,652.159999999981));
#14231=CARTESIAN_POINT('Origin',(32.0000000000012,0.,645.809999999981));
#14232=CARTESIAN_POINT('Origin',(134.030507120984,66.,0.));
#14233=CARTESIAN_POINT('',(134.030507120984,66.,0.));
#14234=CARTESIAN_POINT('',(134.030507120984,66.,0.127016653792582));
#14235=CARTESIAN_POINT('',(134.030507120984,66.,0.));
#14236=CARTESIAN_POINT('',(134.030507120984,69.,4.));
#14237=CARTESIAN_POINT('Origin',(134.030507120984,65.,4.));
#14238=CARTESIAN_POINT('',(134.030507120984,69.,1.83697019872103E-16));
#14239=CARTESIAN_POINT('',(134.030507120984,69.,685.31));
#14240=CARTESIAN_POINT('',(134.030507120984,69.,0.));
#14241=CARTESIAN_POINT('Origin',(4.,66.,4.));
#14242=CARTESIAN_POINT('',(4.,69.,4.));
#14243=CARTESIAN_POINT('',(4.,69.,1.83697019872103E-16));
#14244=CARTESIAN_POINT('',(4.00000000000059,69.,685.31));
#14245=CARTESIAN_POINT('',(4.,66.,0.127016653792582));
#14246=CARTESIAN_POINT('Origin',(4.,65.,4.));
#14247=CARTESIAN_POINT('',(4.,66.,0.));
#14248=CARTESIAN_POINT('',(4.,66.,4.));
#14249=CARTESIAN_POINT('',(4.,66.,0.));
#14250=CARTESIAN_POINT('Origin',(0.,69.,685.31));
#14251=CARTESIAN_POINT('',(134.030507120984,68.9999999999999,681.31));
#14252=CARTESIAN_POINT('',(134.030507120984,69.,685.31));
#14253=CARTESIAN_POINT('',(134.030507120984,69.,4.));
#14254=CARTESIAN_POINT('',(4.,68.9999999999999,681.31));
#14255=CARTESIAN_POINT('',(4.,69.,685.31));
#14256=CARTESIAN_POINT('',(4.,68.9999999999999,681.31));
#14257=CARTESIAN_POINT('Origin',(0.,66.,685.31));
#14258=CARTESIAN_POINT('',(134.030507120984,66.,4.));
#14259=CARTESIAN_POINT('',(4.,66.,4.));
#14260=CARTESIAN_POINT('',(134.030507120984,66.,4.));
#14261=CARTESIAN_POINT('',(134.030507120984,66.,681.31));
#14262=CARTESIAN_POINT('',(134.030507120984,66.,685.31));
#14263=CARTESIAN_POINT('',(4.,65.9999999999999,681.31));
#14264=CARTESIAN_POINT('',(4.,65.9999999999999,681.31));
#14265=CARTESIAN_POINT('',(4.,66.,685.31));
#14266=CARTESIAN_POINT('Origin',(4.,66.,685.31));
#14267=CARTESIAN_POINT('',(4.,66.,685.31));
#14268=CARTESIAN_POINT('',(4.,66.,685.182983346207));
#14269=CARTESIAN_POINT('',(4.,66.,685.31));
#14270=CARTESIAN_POINT('Origin',(4.,64.9999999999999,681.31));
#14271=CARTESIAN_POINT('',(4.,69.,685.31));
#14272=CARTESIAN_POINT('',(4.,69.,685.31));
#14273=CARTESIAN_POINT('',(4.,69.,685.31));
#14274=CARTESIAN_POINT('Origin',(134.030507120984,65.9999999999999,681.31));
#14275=CARTESIAN_POINT('',(134.030507120984,69.,685.31));
#14276=CARTESIAN_POINT('',(134.030507120984,69.,685.31));
#14277=CARTESIAN_POINT('',(134.030507120984,66.,685.182983346207));
#14278=CARTESIAN_POINT('Origin',(134.030507120984,64.9999999999999,681.31));
#14279=CARTESIAN_POINT('',(134.030507120984,66.,685.31));
#14280=CARTESIAN_POINT('',(134.030507120984,66.,685.31));
#14281=CARTESIAN_POINT('',(134.030507120984,66.,685.31));
#14282=CARTESIAN_POINT('Origin',(0.,4.,685.31));
#14283=CARTESIAN_POINT('',(0.,4.,685.31));
#14284=CARTESIAN_POINT('',(3.,4.,685.31));
#14285=CARTESIAN_POINT('',(0.,4.,685.31));
#14286=CARTESIAN_POINT('',(4.,0.,685.31));
#14287=CARTESIAN_POINT('Origin',(4.,4.,685.31));
#14288=CARTESIAN_POINT('',(4.,3.,685.31));
#14289=CARTESIAN_POINT('',(4.,3.,685.31));
#14290=CARTESIAN_POINT('Origin',(4.,4.,685.31));
#14291=CARTESIAN_POINT('Origin',(4.,3.,685.31));
#14292=CARTESIAN_POINT('',(0.,65.,685.31));
#14293=CARTESIAN_POINT('',(0.,0.,685.31));
#14294=CARTESIAN_POINT('',(3.,65.,685.31));
#14295=CARTESIAN_POINT('',(3.,0.,685.31));
#14296=CARTESIAN_POINT('',(3.,65.,685.31));
#14297=CARTESIAN_POINT('Origin',(4.,0.,0.));
#14298=CARTESIAN_POINT('',(4.,0.,0.));
#14299=CARTESIAN_POINT('',(4.,3.,0.));
#14300=CARTESIAN_POINT('',(4.,0.,0.));
#14301=CARTESIAN_POINT('',(0.,4.,0.));
#14302=CARTESIAN_POINT('Origin',(4.,4.,0.));
#14303=CARTESIAN_POINT('',(3.,4.,0.));
#14304=CARTESIAN_POINT('',(3.,4.,0.));
#14305=CARTESIAN_POINT('Origin',(4.,4.,0.));
#14306=CARTESIAN_POINT('Origin',(3.,4.,0.));
#14307=CARTESIAN_POINT('',(60.,0.,0.));
#14308=CARTESIAN_POINT('',(0.,0.,0.));
#14309=CARTESIAN_POINT('',(60.,3.,0.));
#14310=CARTESIAN_POINT('',(0.,3.,0.));
#14311=CARTESIAN_POINT('',(60.,3.,0.));
#14312=CARTESIAN_POINT('Origin',(4.,69.,685.31));
#14313=CARTESIAN_POINT('Origin',(4.,65.,685.31));
#14314=CARTESIAN_POINT('Origin',(4.,65.,685.31));
#14315=CARTESIAN_POINT('Origin',(0.,65.,0.));
#14316=CARTESIAN_POINT('',(0.,65.,0.));
#14317=CARTESIAN_POINT('',(3.,65.,0.));
#14318=CARTESIAN_POINT('',(0.,65.,0.));
#14319=CARTESIAN_POINT('Origin',(4.,65.,0.));
#14320=CARTESIAN_POINT('Origin',(4.,65.,0.));
#14321=CARTESIAN_POINT('Origin',(4.,66.,0.));
#14322=CARTESIAN_POINT('',(0.,0.,0.));
#14323=CARTESIAN_POINT('',(3.,0.,0.));
#14324=CARTESIAN_POINT('Origin',(135.86190766147,68.5561175543429,685.31));
#14325=CARTESIAN_POINT('',(135.86190766147,68.5561175543429,685.31));
#14326=CARTESIAN_POINT('',(134.488357256105,65.8890293885857,685.31));
#14327=CARTESIAN_POINT('',(135.86190766147,68.5561175543429,685.31));
#14328=CARTESIAN_POINT('Origin',(134.030507120984,65.,685.31));
#14329=CARTESIAN_POINT('Origin',(134.030507120984,65.,685.31));
#14330=CARTESIAN_POINT('Origin',(134.030507120984,66.,685.31));
#14331=CARTESIAN_POINT('',(192.831400540487,39.2168287216494,685.31));
#14332=CARTESIAN_POINT('',(135.,69.,685.31));
#14333=CARTESIAN_POINT('',(191.457850135122,36.5497405558923,685.31));
#14334=CARTESIAN_POINT('',(133.626449594635,66.3329118342429,685.31));
#14335=CARTESIAN_POINT('',(191.457850135122,36.5497405558923,685.31));
#14336=CARTESIAN_POINT('Origin',(134.030507120984,69.,0.));
#14337=CARTESIAN_POINT('',(135.86190766147,68.5561175543429,0.));
#14338=CARTESIAN_POINT('Origin',(134.030507120984,65.,0.));
#14339=CARTESIAN_POINT('',(134.488357256105,65.8890293885857,0.));
#14340=CARTESIAN_POINT('',(134.488357256105,65.8890293885857,0.));
#14341=CARTESIAN_POINT('Origin',(134.030507120984,65.,0.));
#14342=CARTESIAN_POINT('Origin',(195.,35.6607111673066,685.31));
#14343=CARTESIAN_POINT('',(195.,35.6607111673066,685.31));
#14344=CARTESIAN_POINT('',(192.,35.6607111673066,685.31));
#14345=CARTESIAN_POINT('',(195.,35.6607111673066,685.31));
#14346=CARTESIAN_POINT('Origin',(191.,35.6607111673066,685.31));
#14347=CARTESIAN_POINT('Origin',(191.,35.6607111673066,685.31));
#14348=CARTESIAN_POINT('Origin',(191.457850135122,36.5497405558923,685.31));
#14349=CARTESIAN_POINT('',(195.,4.00000000000003,685.31));
#14350=CARTESIAN_POINT('',(195.,38.1,685.31));
#14351=CARTESIAN_POINT('',(192.,4.00000000000001,685.31));
#14352=CARTESIAN_POINT('',(192.,38.1,685.31));
#14353=CARTESIAN_POINT('',(192.,4.00000000000001,685.31));
#14354=CARTESIAN_POINT('Origin',(192.831400540487,39.2168287216494,0.));
#14355=CARTESIAN_POINT('',(192.831400540487,39.2168287216494,0.));
#14356=CARTESIAN_POINT('',(191.457850135122,36.5497405558923,0.));
#14357=CARTESIAN_POINT('',(192.831400540487,39.2168287216494,0.));
#14358=CARTESIAN_POINT('',(195.,35.6607111673066,0.));
#14359=CARTESIAN_POINT('Origin',(191.,35.6607111673066,0.));
#14360=CARTESIAN_POINT('',(192.,35.6607111673066,0.));
#14361=CARTESIAN_POINT('',(192.,35.6607111673066,0.));
#14362=CARTESIAN_POINT('Origin',(191.,35.6607111673066,0.));
#14363=CARTESIAN_POINT('Origin',(192.,35.6607111673066,0.));
#14364=CARTESIAN_POINT('',(135.,69.,0.));
#14365=CARTESIAN_POINT('',(133.626449594635,66.3329118342429,0.));
#14366=CARTESIAN_POINT('Origin',(191.,-4.89858719658945E-16,685.31));
#14367=CARTESIAN_POINT('',(191.,-4.89858719658945E-16,685.31));
#14368=CARTESIAN_POINT('',(191.,3.,685.31));
#14369=CARTESIAN_POINT('',(191.,-4.89858719658945E-16,685.31));
#14370=CARTESIAN_POINT('Origin',(191.,4.00000000000001,685.31));
#14371=CARTESIAN_POINT('Origin',(191.,4.00000000000001,685.31));
#14372=CARTESIAN_POINT('Origin',(192.,4.00000000000001,685.31));
#14373=CARTESIAN_POINT('',(160.,-4.28626379701574E-15,685.31));
#14374=CARTESIAN_POINT('',(195.,-3.08148791101958E-30,685.31));
#14375=CARTESIAN_POINT('',(160.,3.,685.31));
#14376=CARTESIAN_POINT('',(195.,3.,685.31));
#14377=CARTESIAN_POINT('',(160.,-4.28626379701574E-15,685.31));
#14378=CARTESIAN_POINT('Origin',(195.,4.00000000000003,0.));
#14379=CARTESIAN_POINT('',(195.,4.00000000000003,0.));
#14380=CARTESIAN_POINT('',(192.,4.00000000000001,0.));
#14381=CARTESIAN_POINT('',(195.,4.00000000000003,0.));
#14382=CARTESIAN_POINT('',(191.,-4.89858719658945E-16,0.));
#14383=CARTESIAN_POINT('Origin',(191.,4.00000000000001,0.));
#14384=CARTESIAN_POINT('',(191.,3.,0.));
#14385=CARTESIAN_POINT('',(191.,3.,0.));
#14386=CARTESIAN_POINT('Origin',(191.,4.00000000000001,0.));
#14387=CARTESIAN_POINT('Origin',(191.,3.,0.));
#14388=CARTESIAN_POINT('',(195.,38.1,0.));
#14389=CARTESIAN_POINT('',(192.,38.1,0.));
#14390=CARTESIAN_POINT('Origin',(195.,3.,685.31));
#14391=CARTESIAN_POINT('',(160.,3.,0.));
#14392=CARTESIAN_POINT('',(195.,3.,0.));
#14393=CARTESIAN_POINT('',(160.,3.,685.31));
#14394=CARTESIAN_POINT('',(191.,3.,685.31));
#14395=CARTESIAN_POINT('Origin',(160.,-4.28626379701574E-15,685.31));
#14396=CARTESIAN_POINT('',(160.,-4.28626379701574E-15,0.));
#14397=CARTESIAN_POINT('',(160.,-4.28626379701574E-15,0.));
#14398=CARTESIAN_POINT('',(160.,-4.28626379701574E-15,685.31));
#14399=CARTESIAN_POINT('Origin',(195.,-3.08148791101958E-30,685.31));
#14400=CARTESIAN_POINT('',(195.,-3.08148791101958E-30,0.));
#14401=CARTESIAN_POINT('',(191.,-4.89858719658945E-16,685.31));
#14402=CARTESIAN_POINT('Origin',(191.,4.00000000000001,685.31));
#14403=CARTESIAN_POINT('',(195.,4.00000000000003,685.31));
#14404=CARTESIAN_POINT('Origin',(195.,38.1,685.31));
#14405=CARTESIAN_POINT('',(195.,35.6607111673066,685.31));
#14406=CARTESIAN_POINT('Origin',(191.,35.6607111673066,685.31));
#14407=CARTESIAN_POINT('',(192.831400540487,39.2168287216494,685.31));
#14408=CARTESIAN_POINT('Origin',(135.,69.,685.31));
#14409=CARTESIAN_POINT('',(135.86190766147,68.5561175543429,685.31));
#14410=CARTESIAN_POINT('Origin',(134.030507120984,65.,685.31));
#14411=CARTESIAN_POINT('Origin',(4.,65.,685.31));
#14412=CARTESIAN_POINT('',(0.,65.,685.31));
#14413=CARTESIAN_POINT('Origin',(0.,0.,685.31));
#14414=CARTESIAN_POINT('',(0.,4.,685.31));
#14415=CARTESIAN_POINT('Origin',(4.,4.,685.31));
#14416=CARTESIAN_POINT('',(4.,0.,685.31));
#14417=CARTESIAN_POINT('Origin',(0.,0.,685.31));
#14418=CARTESIAN_POINT('',(60.,0.,685.31));
#14419=CARTESIAN_POINT('',(60.,0.,685.31));
#14420=CARTESIAN_POINT('',(0.,0.,685.31));
#14421=CARTESIAN_POINT('Origin',(60.,3.,685.31));
#14422=CARTESIAN_POINT('',(60.,3.,685.31));
#14423=CARTESIAN_POINT('',(60.,3.,685.31));
#14424=CARTESIAN_POINT('',(60.,3.,685.31));
#14425=CARTESIAN_POINT('Origin',(0.,3.,685.31));
#14426=CARTESIAN_POINT('',(4.,3.,685.31));
#14427=CARTESIAN_POINT('',(0.,3.,685.31));
#14428=CARTESIAN_POINT('Origin',(4.,4.,685.31));
#14429=CARTESIAN_POINT('',(3.,4.,685.31));
#14430=CARTESIAN_POINT('Origin',(3.,0.,685.31));
#14431=CARTESIAN_POINT('',(3.,65.,685.31));
#14432=CARTESIAN_POINT('Origin',(4.,65.,685.31));
#14433=CARTESIAN_POINT('',(4.,66.,4.));
#14434=CARTESIAN_POINT('',(4.,66.,685.31));
#14435=CARTESIAN_POINT('Origin',(134.030507120984,65.,685.31));
#14436=CARTESIAN_POINT('',(134.488357256105,65.8890293885857,685.31));
#14437=CARTESIAN_POINT('',(134.030507120984,66.,685.31));
#14438=CARTESIAN_POINT('',(134.030507120984,66.,0.));
#14439=CARTESIAN_POINT('Origin',(133.626449594635,66.3329118342429,685.31));
#14440=CARTESIAN_POINT('',(191.457850135122,36.5497405558923,685.31));
#14441=CARTESIAN_POINT('Origin',(191.,35.6607111673066,685.31));
#14442=CARTESIAN_POINT('',(192.,35.6607111673066,685.31));
#14443=CARTESIAN_POINT('Origin',(192.,38.1,685.31));
#14444=CARTESIAN_POINT('',(192.,4.00000000000001,685.31));
#14445=CARTESIAN_POINT('Origin',(191.,4.00000000000001,685.31));
#14446=CARTESIAN_POINT('Origin',(191.,4.00000000000001,685.31));
#14447=CARTESIAN_POINT('Origin',(191.,4.00000000000001,0.));
#14448=CARTESIAN_POINT('Origin',(134.030507120984,64.9999999999999,681.31));
#14449=CARTESIAN_POINT('',(134.030507120984,64.9999999999999,685.31));
#14450=CARTESIAN_POINT('Origin',(134.030507120984,64.9999999999999,681.31));
#14451=CARTESIAN_POINT('',(134.030507120984,64.9999999999999,682.31));
#14452=CARTESIAN_POINT('',(134.030507120984,64.9999999999999,685.31));
#14453=CARTESIAN_POINT('Origin',(134.030507120984,64.9999999999999,681.31));
#14454=CARTESIAN_POINT('Origin',(4.,64.9999999999999,681.31));
#14455=CARTESIAN_POINT('',(4.,64.9999999999999,685.31));
#14456=CARTESIAN_POINT('Origin',(4.,64.9999999999999,681.31));
#14457=CARTESIAN_POINT('',(4.,64.9999999999999,682.31));
#14458=CARTESIAN_POINT('Origin',(4.,64.9999999999999,681.31));
#14459=CARTESIAN_POINT('',(4.,64.9999999999999,682.31));
#14460=CARTESIAN_POINT('Origin',(4.,64.9999999999999,681.31));
#14461=CARTESIAN_POINT('',(134.030507120984,64.9999999999999,685.31));
#14462=CARTESIAN_POINT('Origin',(4.,64.9999999999999,681.31));
#14463=CARTESIAN_POINT('',(134.030507120984,64.9999999999999,682.31));
#14464=CARTESIAN_POINT('Origin',(4.,9.00000000000001,685.31));
#14465=CARTESIAN_POINT('',(4.,8.99999999999999,682.31));
#14466=CARTESIAN_POINT('',(4.,8.99999999999999,682.31));
#14467=CARTESIAN_POINT('',(4.,9.00000000000001,685.31));
#14468=CARTESIAN_POINT('',(4.,9.00000000000001,685.31));
#14469=CARTESIAN_POINT('',(4.,2.6801128335108E-12,685.31));
#14470=CARTESIAN_POINT('Origin',(134.030507120984,66.,685.31));
#14471=CARTESIAN_POINT('',(134.030507120984,61.3121699873772,685.31));
#14472=CARTESIAN_POINT('',(134.030507120984,2.6801128335108E-12,685.31));
#14473=CARTESIAN_POINT('',(134.030507120984,61.3121699873772,682.31));
#14474=CARTESIAN_POINT('',(134.030507120984,61.3121699873772,682.31));
#14475=CARTESIAN_POINT('',(134.030507120984,66.,682.31));
#14476=CARTESIAN_POINT('Origin',(0.,2.6801128335108E-12,685.31));
#14477=CARTESIAN_POINT('',(187.353206910234,9.00000000000001,685.31));
#14478=CARTESIAN_POINT('',(0.,9.00000000000001,685.31));
#14479=CARTESIAN_POINT('',(187.353206910234,33.8509795959131,685.31));
#14480=CARTESIAN_POINT('',(187.353206910234,9.00000000000001,685.31));
#14481=CARTESIAN_POINT('',(187.353206910234,33.8509795959131,685.31));
#14482=CARTESIAN_POINT('Origin',(0.,2.66963838949427E-12,682.31));
#14483=CARTESIAN_POINT('',(187.353206910234,33.8509795959131,682.31));
#14484=CARTESIAN_POINT('',(187.353206910234,33.8509795959131,682.31));
#14485=CARTESIAN_POINT('',(187.353206910234,9.00000000000001,682.31));
#14486=CARTESIAN_POINT('',(187.353206910234,9.00000000000001,682.31));
#14487=CARTESIAN_POINT('',(134.030507120984,8.99999999999999,682.31));
#14488=CARTESIAN_POINT('Origin',(134.030507120984,9.00000000000001,685.31));
#14489=CARTESIAN_POINT('',(187.353206910234,9.00000000000001,682.31));
#14490=CARTESIAN_POINT('Origin',(187.353206910234,33.8509795959131,682.31));
#14491=CARTESIAN_POINT('',(187.353206910234,33.8509795959131,682.31));
#14492=CARTESIAN_POINT('Origin',(187.353206910234,9.00000000000001,682.31));
#14493=CARTESIAN_POINT('Origin',(4.,65.,4.));
#14494=CARTESIAN_POINT('',(4.,65.,3.));
#14495=CARTESIAN_POINT('Origin',(4.,65.,4.));
#14496=CARTESIAN_POINT('',(4.,65.,-1.73472347597681E-15));
#14497=CARTESIAN_POINT('Origin',(4.,65.,4.));
#14498=CARTESIAN_POINT('',(4.,65.,-6.98296267768613E-15));
#14499=CARTESIAN_POINT('Origin',(134.030507120984,65.,4.));
#14500=CARTESIAN_POINT('',(134.030507120984,65.,-3.328228599496E-15));
#14501=CARTESIAN_POINT('Origin',(134.030507120984,65.,4.));
#14502=CARTESIAN_POINT('',(134.030507120984,65.,3.));
#14503=CARTESIAN_POINT('Origin',(134.030507120984,65.,4.));
#14504=CARTESIAN_POINT('',(134.030507120984,65.,3.));
#14505=CARTESIAN_POINT('Origin',(134.030507120984,65.,4.));
#14506=CARTESIAN_POINT('',(4.,65.,-3.46944695195361E-15));
#14507=CARTESIAN_POINT('Origin',(134.030507120984,65.,4.));
#14508=CARTESIAN_POINT('',(4.,65.,3.));
#14509=CARTESIAN_POINT('Origin',(4.,66.,0.));
#14510=CARTESIAN_POINT('',(4.,9.00000000000001,-1.98861209386333E-13));
#14511=CARTESIAN_POINT('',(4.,1.04744440165302E-14,-2.30284541435921E-13));
#14512=CARTESIAN_POINT('',(4.,8.99999999999999,2.9999999999998));
#14513=CARTESIAN_POINT('',(4.,9.00000000000001,-1.99014436314059E-13));
#14514=CARTESIAN_POINT('',(4.,66.,3.));
#14515=CARTESIAN_POINT('Origin',(134.030507120984,9.00000000000001,-1.99059518868339E-13));
#14516=CARTESIAN_POINT('',(134.030507120984,61.3121699873795,3.00000000000021));
#14517=CARTESIAN_POINT('',(134.030507120984,8.99999999999999,2.9999999999998));
#14518=CARTESIAN_POINT('',(134.030507120984,61.3121699873796,2.14070297354914E-13));
#14519=CARTESIAN_POINT('',(134.030507120984,61.3121699873795,3.00000000000021));
#14520=CARTESIAN_POINT('',(134.030507120984,1.04744440165302E-14,-2.30284541435921E-13));
#14521=CARTESIAN_POINT('Origin',(0.,1.04744440165302E-14,-2.30284541435921E-13));
#14522=CARTESIAN_POINT('',(187.353206910234,33.8509795959155,1.18190063560699E-13));
#14523=CARTESIAN_POINT('',(134.030507120984,61.3121699873796,2.14070297354914E-13));
#14524=CARTESIAN_POINT('',(187.353206910234,9.0000000000024,3.14233320495966E-14));
#14525=CARTESIAN_POINT('',(187.353206910234,33.8509795959155,1.18190063560699E-13));
#14526=CARTESIAN_POINT('',(0.,9.00000000000001,-1.98861209386333E-13));
#14527=CARTESIAN_POINT('Origin',(0.,8.04569168006329E-28,2.99999999999977));
#14528=CARTESIAN_POINT('',(187.353206910234,9.00000000000239,3.00000000000003));
#14529=CARTESIAN_POINT('',(4.,8.99999999999999,2.9999999999998));
#14530=CARTESIAN_POINT('',(187.353206910234,33.8509795959155,3.00000000000012));
#14531=CARTESIAN_POINT('',(187.353206910234,33.8509795959155,3.00000000000012));
#14532=CARTESIAN_POINT('',(134.030507120984,61.3121699873795,3.00000000000021));
#14533=CARTESIAN_POINT('Origin',(4.,9.00000000000001,-1.99059518868339E-13));
#14534=CARTESIAN_POINT('',(187.353206910234,9.00000000000239,3.00000000000003));
#14535=CARTESIAN_POINT('Origin',(187.353206910234,33.8509795959155,3.00000000000012));
#14536=CARTESIAN_POINT('',(187.353206910234,33.8509795959155,3.00000000000012));
#14537=CARTESIAN_POINT('Origin',(134.030507120984,61.3121699873795,3.00000000000021));
#14538=CARTESIAN_POINT('',(0.,0.,0.));
#14539=CARTESIAN_POINT('Origin',(-81.58,34.5,63.9999999999928));
#14540=CARTESIAN_POINT('',(-82.,34.5,57.6500000012826));
#14541=CARTESIAN_POINT('Origin',(-82.,34.5,63.9999999999928));
#14542=CARTESIAN_POINT('',(-85.,34.5,57.6500000012826));
#14543=CARTESIAN_POINT('',(-81.58,34.5,57.6500000012826));
#14544=CARTESIAN_POINT('Origin',(-85.,34.5,63.9999999999928));
#14545=CARTESIAN_POINT('Origin',(-81.58,34.5,138.999999999993));
#14546=CARTESIAN_POINT('',(-82.,34.5,132.650000001283));
#14547=CARTESIAN_POINT('Origin',(-82.,34.5,138.999999999993));
#14548=CARTESIAN_POINT('',(-85.,34.5,132.650000001283));
#14549=CARTESIAN_POINT('',(-81.58,34.5,132.650000001283));
#14550=CARTESIAN_POINT('Origin',(-85.,34.5,138.999999999993));
#14551=CARTESIAN_POINT('Origin',(-81.58,37.8359855953527,608.));
#14552=CARTESIAN_POINT('',(-82.,37.8359855953527,601.65));
#14553=CARTESIAN_POINT('Origin',(-82.,37.8359855953527,608.));
#14554=CARTESIAN_POINT('',(-85.,37.8359855953527,601.65));
#14555=CARTESIAN_POINT('',(-81.58,37.8359855953527,601.65));
#14556=CARTESIAN_POINT('Origin',(-85.,37.8359855953527,608.));
#14557=CARTESIAN_POINT('Origin',(-81.58,35.9826602646012,683.));
#14558=CARTESIAN_POINT('',(-82.,35.9826602646012,676.019466760152));
#14559=CARTESIAN_POINT('Origin',(-82.,35.9826602646012,683.));
#14560=CARTESIAN_POINT('',(-85.,35.9826602646012,676.019466760152));
#14561=CARTESIAN_POINT('',(-81.58,35.9826602646012,676.019466760152));
#14562=CARTESIAN_POINT('Origin',(-85.,35.9826602646012,683.));
#14563=CARTESIAN_POINT('Origin',(-42.5,1.49999999999999,32.0000000000144));
#14564=CARTESIAN_POINT('',(-48.85,-6.10622663543836E-15,32.0000000000144));
#14565=CARTESIAN_POINT('Origin',(-42.5,-5.20417042793042E-15,32.0000000000144));
#14566=CARTESIAN_POINT('',(-48.85,-3.00000000000001,32.0000000000144));
#14567=CARTESIAN_POINT('',(-48.85,1.49999999999999,32.0000000000144));
#14568=CARTESIAN_POINT('Origin',(-42.5,-3.00000000000001,32.0000000000144));
#14569=CARTESIAN_POINT('Origin',(-42.5000000000001,1.49999999999999,713.999999999986));
#14570=CARTESIAN_POINT('',(-48.8500000000001,-6.10622663543836E-15,713.999999999986));
#14571=CARTESIAN_POINT('Origin',(-42.5000000000001,-5.20417042793042E-15,
713.999999999986));
#14572=CARTESIAN_POINT('',(-48.8500000000001,-3.00000000000001,713.999999999986));
#14573=CARTESIAN_POINT('',(-48.8500000000001,1.49999999999999,713.999999999986));
#14574=CARTESIAN_POINT('Origin',(-42.5000000000001,-3.00000000000001,713.999999999986));
#14575=CARTESIAN_POINT('Origin',(-42.2900000000001,1.49999999999999,529.5));
#14576=CARTESIAN_POINT('',(-48.6400000000001,-6.10622663543836E-15,529.5));
#14577=CARTESIAN_POINT('Origin',(-42.2900000000001,-5.20417042793042E-15,
529.5));
#14578=CARTESIAN_POINT('',(-48.6400000000001,-3.00000000000001,529.5));
#14579=CARTESIAN_POINT('',(-48.6400000000001,1.49999999999999,529.5));
#14580=CARTESIAN_POINT('Origin',(-42.2900000000001,-3.00000000000001,529.5));
#14581=CARTESIAN_POINT('Origin',(-42.5,1.49999999999999,175.500000000014));
#14582=CARTESIAN_POINT('',(-48.85,-6.10622663543836E-15,175.500000000014));
#14583=CARTESIAN_POINT('Origin',(-42.5,-5.20417042793042E-15,175.500000000014));
#14584=CARTESIAN_POINT('',(-48.85,-3.00000000000001,175.500000000014));
#14585=CARTESIAN_POINT('',(-48.85,1.49999999999999,175.500000000014));
#14586=CARTESIAN_POINT('Origin',(-42.5,-3.00000000000001,175.500000000014));
#14587=CARTESIAN_POINT('Origin',(-85.,68.,0.));
#14588=CARTESIAN_POINT('',(-81.,72.,0.));
#14589=CARTESIAN_POINT('',(-33.5,72.,0.));
#14590=CARTESIAN_POINT('',(-82.,72.,0.));
#14591=CARTESIAN_POINT('',(-33.5,69.,0.));
#14592=CARTESIAN_POINT('',(-33.5,68.,0.));
#14593=CARTESIAN_POINT('',(-81.,69.,0.));
#14594=CARTESIAN_POINT('',(-82.,69.,0.));
#14595=CARTESIAN_POINT('',(-81.,69.,0.));
#14596=CARTESIAN_POINT('Origin',(-81.,-9.91963907309357E-15,746.));
#14597=CARTESIAN_POINT('',(-81.,-9.91963907309357E-15,746.));
#14598=CARTESIAN_POINT('',(-81.,-3.00000000000001,746.));
#14599=CARTESIAN_POINT('',(-81.,-9.91963907309357E-15,746.));
#14600=CARTESIAN_POINT('',(-82.,0.99999999999999,746.));
#14601=CARTESIAN_POINT('Origin',(-81.,0.99999999999999,746.));
#14602=CARTESIAN_POINT('',(-85.,0.99999999999999,746.));
#14603=CARTESIAN_POINT('',(-85.,0.99999999999999,746.));
#14604=CARTESIAN_POINT('Origin',(-81.,0.99999999999999,746.));
#14605=CARTESIAN_POINT('Origin',(-85.,0.99999999999999,746.));
#14606=CARTESIAN_POINT('',(0.,0.,746.));
#14607=CARTESIAN_POINT('',(0.,0.,746.));
#14608=CARTESIAN_POINT('',(3.67394039744206E-16,-3.,746.));
#14609=CARTESIAN_POINT('',(3.67394039744206E-16,-3.,746.));
#14610=CARTESIAN_POINT('',(0.,0.,746.));
#14611=CARTESIAN_POINT('Origin',(-82.,0.99999999999999,0.));
#14612=CARTESIAN_POINT('',(-82.,0.99999999999999,0.));
#14613=CARTESIAN_POINT('',(-85.,0.99999999999999,0.));
#14614=CARTESIAN_POINT('',(-82.,0.99999999999999,0.));
#14615=CARTESIAN_POINT('',(-81.,-9.91963907309357E-15,0.));
#14616=CARTESIAN_POINT('Origin',(-81.,0.99999999999999,0.));
#14617=CARTESIAN_POINT('',(-81.,-3.00000000000001,0.));
#14618=CARTESIAN_POINT('',(-81.,-3.00000000000001,0.));
#14619=CARTESIAN_POINT('Origin',(-81.,0.99999999999999,0.));
#14620=CARTESIAN_POINT('Origin',(-81.,-3.00000000000001,0.));
#14621=CARTESIAN_POINT('',(-82.,68.,0.));
#14622=CARTESIAN_POINT('',(-82.,-1.00421037530083E-14,0.));
#14623=CARTESIAN_POINT('',(-85.,68.,0.));
#14624=CARTESIAN_POINT('',(-85.,-1.00421037530083E-14,0.));
#14625=CARTESIAN_POINT('',(-85.,68.,0.));
#14626=CARTESIAN_POINT('Origin',(-82.,68.,746.));
#14627=CARTESIAN_POINT('',(-82.,68.,746.));
#14628=CARTESIAN_POINT('',(-85.,68.,746.));
#14629=CARTESIAN_POINT('',(-82.,68.,746.));
#14630=CARTESIAN_POINT('',(-81.,69.,746.));
#14631=CARTESIAN_POINT('Origin',(-81.,68.,746.));
#14632=CARTESIAN_POINT('',(-81.,72.,746.));
#14633=CARTESIAN_POINT('',(-81.,72.,746.));
#14634=CARTESIAN_POINT('Origin',(-81.,68.,746.));
#14635=CARTESIAN_POINT('Origin',(-81.,72.,746.));
#14636=CARTESIAN_POINT('',(-82.,-1.00421037530083E-14,746.));
#14637=CARTESIAN_POINT('',(-85.,-1.00421037530083E-14,746.));
#14638=CARTESIAN_POINT('Origin',(-81.,69.,0.));
#14639=CARTESIAN_POINT('Origin',(-81.,68.,0.));
#14640=CARTESIAN_POINT('Origin',(-81.,68.,0.));
#14641=CARTESIAN_POINT('Origin',(-29.,68.,746.));
#14642=CARTESIAN_POINT('',(-33.5,72.,746.));
#14643=CARTESIAN_POINT('',(-33.5,69.,746.));
#14644=CARTESIAN_POINT('',(-33.5,50.,746.));
#14645=CARTESIAN_POINT('',(-82.,72.,746.));
#14646=CARTESIAN_POINT('',(-82.,69.,746.));
#14647=CARTESIAN_POINT('Origin',(-32.,69.,746.));
#14648=CARTESIAN_POINT('',(-32.,68.,565.447580013871));
#14649=CARTESIAN_POINT('',(-32.,68.,139.329431198143));
#14650=CARTESIAN_POINT('',(-32.,68.,746.));
#14651=CARTESIAN_POINT('',(-32.,50.,173.817851090086));
#14652=CARTESIAN_POINT('',(-32.0000000000001,-180.631730474111,615.713626701011));
#14653=CARTESIAN_POINT('',(-32.,50.,531.514786028642));
#14654=CARTESIAN_POINT('',(-32.,50.,746.));
#14655=CARTESIAN_POINT('',(-32.,142.963452937836,706.765324733926));
#14656=CARTESIAN_POINT('Origin',(-29.,50.,746.));
#14657=CARTESIAN_POINT('',(-29.,50.,173.817851090086));
#14658=CARTESIAN_POINT('',(-33.5,50.,173.817851090086));
#14659=CARTESIAN_POINT('',(-29.,50.,531.514786028642));
#14660=CARTESIAN_POINT('',(-29.,50.,746.));
#14661=CARTESIAN_POINT('',(-33.5,50.,531.514786028642));
#14662=CARTESIAN_POINT('Origin',(-29.,69.,746.));
#14663=CARTESIAN_POINT('',(-29.,68.,139.329431198143));
#14664=CARTESIAN_POINT('',(-29.,50.,173.817851090086));
#14665=CARTESIAN_POINT('',(-29.,68.,565.447580013871));
#14666=CARTESIAN_POINT('',(-29.,68.,746.));
#14667=CARTESIAN_POINT('',(-29.,72.6655742581807,574.242911687517));
#14668=CARTESIAN_POINT('Origin',(-33.,68.,746.));
#14669=CARTESIAN_POINT('',(-33.,72.,131.665337888822));
#14670=CARTESIAN_POINT('Origin',(-33.0000000000006,67.9999999999993,139.329431198144));
#14671=CARTESIAN_POINT('',(-33.,72.,572.988200899477));
#14672=CARTESIAN_POINT('',(-33.,72.,746.));
#14673=CARTESIAN_POINT('Origin',(-32.9999999999998,68.0000000000002,565.447580013871));
#14674=CARTESIAN_POINT('Origin',(-82.,72.,746.));
#14675=CARTESIAN_POINT('',(-33.5,72.,131.665337888822));
#14676=CARTESIAN_POINT('',(-82.,72.,131.665337888822));
#14677=CARTESIAN_POINT('',(-33.5,72.,746.));
#14678=CARTESIAN_POINT('',(-81.,72.,746.));
#14679=CARTESIAN_POINT('',(-33.5,72.,572.988200899477));
#14680=CARTESIAN_POINT('',(-33.5,72.,746.));
#14681=CARTESIAN_POINT('',(-82.,72.,572.988200899477));
#14682=CARTESIAN_POINT('Origin',(-81.,68.,746.));
#14683=CARTESIAN_POINT('',(-85.,68.,746.));
#14684=CARTESIAN_POINT('Origin',(-85.,-1.00421037530083E-14,746.));
#14685=CARTESIAN_POINT('',(-85.,0.99999999999999,746.));
#14686=CARTESIAN_POINT('Origin',(-81.,0.99999999999999,746.));
#14687=CARTESIAN_POINT('',(-81.,-3.00000000000001,746.));
#14688=CARTESIAN_POINT('Origin',(3.67394039744206E-16,-3.,746.));
#14689=CARTESIAN_POINT('',(3.67394039744206E-16,-3.,0.));
#14690=CARTESIAN_POINT('',(3.67394039744206E-16,-3.,0.));
#14691=CARTESIAN_POINT('',(3.67394039744206E-16,-3.,746.));
#14692=CARTESIAN_POINT('Origin',(0.,0.,746.));
#14693=CARTESIAN_POINT('',(0.,0.,0.));
#14694=CARTESIAN_POINT('',(0.,0.,0.));
#14695=CARTESIAN_POINT('',(0.,0.,746.));
#14696=CARTESIAN_POINT('Origin',(0.,0.,746.));
#14697=CARTESIAN_POINT('',(0.,0.,0.));
#14698=CARTESIAN_POINT('',(-81.,-9.91963907309357E-15,746.));
#14699=CARTESIAN_POINT('Origin',(-81.,0.99999999999999,746.));
#14700=CARTESIAN_POINT('',(-82.,0.99999999999999,746.));
#14701=CARTESIAN_POINT('Origin',(-82.,-1.00421037530083E-14,746.));
#14702=CARTESIAN_POINT('',(-82.,68.,746.));
#14703=CARTESIAN_POINT('Origin',(-81.,68.,746.));
#14704=CARTESIAN_POINT('',(-81.,69.,746.));
#14705=CARTESIAN_POINT('Origin',(-82.,69.,746.));
#14706=CARTESIAN_POINT('',(-33.5,69.,137.413407870812));
#14707=CARTESIAN_POINT('',(-33.5,69.,746.));
#14708=CARTESIAN_POINT('',(-33.,69.,137.413407870813));
#14709=CARTESIAN_POINT('',(-82.,69.,137.413407870813));
#14710=CARTESIAN_POINT('',(-33.,69.,567.332735235272));
#14711=CARTESIAN_POINT('',(-33.,69.,746.));
#14712=CARTESIAN_POINT('',(-33.5,69.,567.332735235272));
#14713=CARTESIAN_POINT('',(-82.,69.,567.332735235272));
#14714=CARTESIAN_POINT('',(-33.5,69.,746.));
#14715=CARTESIAN_POINT('Origin',(-33.,68.,746.));
#14716=CARTESIAN_POINT('Origin',(-33.0000000000001,67.9999999999998,139.329431198143));
#14717=CARTESIAN_POINT('Origin',(-32.9999999999994,68.0000000000007,565.447580013872));
#14718=CARTESIAN_POINT('Origin',(-33.,68.,0.));
#14719=CARTESIAN_POINT('Origin',(-33.5,0.,0.));
#14720=CARTESIAN_POINT('',(-33.5,72.6655742581807,574.242911687517));
#14721=CARTESIAN_POINT('Origin',(-33.5,72.6655742581807,574.242911687517));
#14722=CARTESIAN_POINT('Origin',(-33.5,50.,173.817851090086));
#14723=CARTESIAN_POINT('',(-33.5,50.,173.817851090086));
#14724=CARTESIAN_POINT('Origin',(-33.5,0.,0.));
#14725=CARTESIAN_POINT('',(0.,0.,0.));
#14726=CARTESIAN_POINT('Origin',(-81.58,34.5,-138.999999999993));
#14727=CARTESIAN_POINT('',(-82.,34.5,-146.110984814694));
#14728=CARTESIAN_POINT('Origin',(-82.,34.5,-138.999999999993));
#14729=CARTESIAN_POINT('',(-85.,34.5,-146.110984814694));
#14730=CARTESIAN_POINT('',(-81.58,34.5,-146.110984814694));
#14731=CARTESIAN_POINT('Origin',(-85.,34.5,-138.999999999993));
#14732=CARTESIAN_POINT('Origin',(-81.58,34.5,-63.9999999999928));
#14733=CARTESIAN_POINT('',(-82.,34.5,-57.6500000012826));
#14734=CARTESIAN_POINT('Origin',(-82.,34.5,-63.9999999999928));
#14735=CARTESIAN_POINT('',(-85.,34.5,-57.6500000012826));
#14736=CARTESIAN_POINT('',(-81.58,34.5,-57.6500000012826));
#14737=CARTESIAN_POINT('Origin',(-85.,34.5,-63.9999999999928));
#14738=CARTESIAN_POINT('Origin',(-81.58,37.8359855953527,-608.));
#14739=CARTESIAN_POINT('',(-82.,37.8359855953527,-601.65));
#14740=CARTESIAN_POINT('Origin',(-82.,37.8359855953527,-608.));
#14741=CARTESIAN_POINT('',(-85.,37.8359855953527,-601.65));
#14742=CARTESIAN_POINT('',(-81.58,37.8359855953527,-601.65));
#14743=CARTESIAN_POINT('Origin',(-85.,37.8359855953527,-608.));
#14744=CARTESIAN_POINT('Origin',(-81.58,35.9826602646012,-683.));
#14745=CARTESIAN_POINT('',(-82.,35.9826602646012,-676.019466760152));
#14746=CARTESIAN_POINT('Origin',(-82.,35.9826602646012,-683.));
#14747=CARTESIAN_POINT('',(-85.,35.9826602646012,-676.019466760152));
#14748=CARTESIAN_POINT('',(-81.58,35.9826602646012,-676.019466760152));
#14749=CARTESIAN_POINT('Origin',(-85.,35.9826602646012,-683.));
#14750=CARTESIAN_POINT('Origin',(-42.5,1.49999999999999,-32.0000000000144));
#14751=CARTESIAN_POINT('',(-48.85,-6.10622663543836E-15,-32.0000000000144));
#14752=CARTESIAN_POINT('Origin',(-42.5,-5.20417042793042E-15,-32.0000000000144));
#14753=CARTESIAN_POINT('',(-48.85,-3.00000000000001,-32.0000000000144));
#14754=CARTESIAN_POINT('',(-48.85,1.49999999999999,-32.0000000000144));
#14755=CARTESIAN_POINT('Origin',(-42.5,-3.00000000000001,-32.0000000000144));
#14756=CARTESIAN_POINT('Origin',(-42.5000000000001,1.49999999999999,-713.999999999986));
#14757=CARTESIAN_POINT('',(-48.8500000000001,-6.10622663543836E-15,-713.999999999986));
#14758=CARTESIAN_POINT('Origin',(-42.5000000000001,-5.20417042793042E-15,
-713.999999999986));
#14759=CARTESIAN_POINT('',(-48.8500000000001,-3.00000000000001,-713.999999999986));
#14760=CARTESIAN_POINT('',(-48.8500000000001,1.49999999999999,-713.999999999986));
#14761=CARTESIAN_POINT('Origin',(-42.5000000000001,-3.00000000000001,-713.999999999986));
#14762=CARTESIAN_POINT('Origin',(-42.2900000000001,1.49999999999999,-529.5));
#14763=CARTESIAN_POINT('',(-48.6400000000001,-6.10622663543836E-15,-529.5));
#14764=CARTESIAN_POINT('Origin',(-42.2900000000001,-5.20417042793042E-15,
-529.5));
#14765=CARTESIAN_POINT('',(-48.6400000000001,-3.00000000000001,-529.5));
#14766=CARTESIAN_POINT('',(-48.6400000000001,1.49999999999999,-529.5));
#14767=CARTESIAN_POINT('Origin',(-42.2900000000001,-3.00000000000001,-529.5));
#14768=CARTESIAN_POINT('Origin',(-42.5,1.49999999999999,-175.500000000014));
#14769=CARTESIAN_POINT('',(-48.85,-6.10622663543836E-15,-175.500000000014));
#14770=CARTESIAN_POINT('Origin',(-42.5,-5.20417042793042E-15,-175.500000000014));
#14771=CARTESIAN_POINT('',(-48.85,-3.00000000000001,-175.500000000014));
#14772=CARTESIAN_POINT('',(-48.85,1.49999999999999,-175.500000000014));
#14773=CARTESIAN_POINT('Origin',(-42.5,-3.00000000000001,-175.500000000014));
#14774=CARTESIAN_POINT('Origin',(-85.,68.,0.));
#14775=CARTESIAN_POINT('',(-81.,72.,0.));
#14776=CARTESIAN_POINT('',(-33.5,72.,0.));
#14777=CARTESIAN_POINT('',(-82.,72.,0.));
#14778=CARTESIAN_POINT('',(-81.,69.,0.));
#14779=CARTESIAN_POINT('',(-81.,69.,0.));
#14780=CARTESIAN_POINT('',(-33.5,69.,0.));
#14781=CARTESIAN_POINT('',(-82.,69.,0.));
#14782=CARTESIAN_POINT('',(-33.5,68.,0.));
#14783=CARTESIAN_POINT('Origin',(-81.,-9.91963907309357E-15,-746.));
#14784=CARTESIAN_POINT('',(-81.,-9.91963907309357E-15,-746.));
#14785=CARTESIAN_POINT('',(-81.,-3.00000000000001,-746.));
#14786=CARTESIAN_POINT('',(-81.,-9.91963907309357E-15,-746.));
#14787=CARTESIAN_POINT('',(-85.,0.99999999999999,-746.));
#14788=CARTESIAN_POINT('Origin',(-81.,0.99999999999999,-746.));
#14789=CARTESIAN_POINT('',(-82.,0.99999999999999,-746.));
#14790=CARTESIAN_POINT('',(-85.,0.99999999999999,-746.));
#14791=CARTESIAN_POINT('Origin',(-81.,0.99999999999999,-746.));
#14792=CARTESIAN_POINT('Origin',(-85.,0.99999999999999,-746.));
#14793=CARTESIAN_POINT('',(0.,0.,-746.));
#14794=CARTESIAN_POINT('',(0.,0.,-746.));
#14795=CARTESIAN_POINT('',(3.67394039744206E-16,-3.,-746.));
#14796=CARTESIAN_POINT('',(0.,0.,-746.));
#14797=CARTESIAN_POINT('',(3.67394039744206E-16,-3.,-746.));
#14798=CARTESIAN_POINT('Origin',(-82.,0.99999999999999,0.));
#14799=CARTESIAN_POINT('',(-82.,0.99999999999999,0.));
#14800=CARTESIAN_POINT('',(-85.,0.99999999999999,0.));
#14801=CARTESIAN_POINT('',(-82.,0.99999999999999,0.));
#14802=CARTESIAN_POINT('',(-81.,-3.00000000000001,0.));
#14803=CARTESIAN_POINT('Origin',(-81.,0.99999999999999,0.));
#14804=CARTESIAN_POINT('',(-81.,-9.91963907309357E-15,0.));
#14805=CARTESIAN_POINT('',(-81.,-3.00000000000001,0.));
#14806=CARTESIAN_POINT('Origin',(-81.,0.99999999999999,0.));
#14807=CARTESIAN_POINT('Origin',(-81.,-3.00000000000001,0.));
#14808=CARTESIAN_POINT('',(-82.,68.,0.));
#14809=CARTESIAN_POINT('',(-82.,-1.00421037530083E-14,0.));
#14810=CARTESIAN_POINT('',(-85.,68.,0.));
#14811=CARTESIAN_POINT('',(-85.,68.,0.));
#14812=CARTESIAN_POINT('',(-85.,-1.00421037530083E-14,0.));
#14813=CARTESIAN_POINT('Origin',(-82.,68.,-746.));
#14814=CARTESIAN_POINT('',(-82.,68.,-746.));
#14815=CARTESIAN_POINT('',(-85.,68.,-746.));
#14816=CARTESIAN_POINT('',(-82.,68.,-746.));
#14817=CARTESIAN_POINT('',(-81.,72.,-746.));
#14818=CARTESIAN_POINT('Origin',(-81.,68.,-746.));
#14819=CARTESIAN_POINT('',(-81.,69.,-746.));
#14820=CARTESIAN_POINT('',(-81.,72.,-746.));
#14821=CARTESIAN_POINT('Origin',(-81.,68.,-746.));
#14822=CARTESIAN_POINT('Origin',(-81.,72.,-746.));
#14823=CARTESIAN_POINT('',(-82.,-1.00421037530083E-14,-746.));
#14824=CARTESIAN_POINT('',(-85.,-1.00421037530083E-14,-746.));
#14825=CARTESIAN_POINT('Origin',(-81.,69.,0.));
#14826=CARTESIAN_POINT('Origin',(-81.,68.,0.));
#14827=CARTESIAN_POINT('Origin',(-81.,68.,0.));
#14828=CARTESIAN_POINT('Origin',(-29.,68.,-746.));
#14829=CARTESIAN_POINT('',(-33.5,72.,-746.));
#14830=CARTESIAN_POINT('',(-33.5,69.,-746.));
#14831=CARTESIAN_POINT('',(-33.5,50.,-746.));
#14832=CARTESIAN_POINT('',(-82.,69.,-746.));
#14833=CARTESIAN_POINT('',(-82.,72.,-746.));
#14834=CARTESIAN_POINT('Origin',(-32.,69.,-746.));
#14835=CARTESIAN_POINT('',(-32.,68.,-565.447580013871));
#14836=CARTESIAN_POINT('',(-32.,68.,-139.329431198143));
#14837=CARTESIAN_POINT('',(-32.,68.,-746.));
#14838=CARTESIAN_POINT('',(-32.,50.,-531.514786028642));
#14839=CARTESIAN_POINT('',(-32.,142.963452937836,-706.765324733926));
#14840=CARTESIAN_POINT('',(-32.,50.,-173.817851090086));
#14841=CARTESIAN_POINT('',(-32.,50.,-746.));
#14842=CARTESIAN_POINT('',(-32.0000000000001,-180.631730474111,-615.713626701011));
#14843=CARTESIAN_POINT('Origin',(-29.,50.,-746.));
#14844=CARTESIAN_POINT('',(-29.,50.,-173.817851090086));
#14845=CARTESIAN_POINT('',(-33.5,50.,-173.817851090086));
#14846=CARTESIAN_POINT('',(-29.,50.,-531.514786028642));
#14847=CARTESIAN_POINT('',(-33.5,50.,-531.514786028642));
#14848=CARTESIAN_POINT('',(-29.,50.,-746.));
#14849=CARTESIAN_POINT('Origin',(-29.,69.,-746.));
#14850=CARTESIAN_POINT('',(-29.,68.,-139.329431198143));
#14851=CARTESIAN_POINT('',(-29.,50.,-173.817851090086));
#14852=CARTESIAN_POINT('',(-29.,68.,-565.447580013871));
#14853=CARTESIAN_POINT('',(-29.,72.6655742581807,-574.242911687517));
#14854=CARTESIAN_POINT('',(-29.,68.,-746.));
#14855=CARTESIAN_POINT('Origin',(-33.,68.,-746.));
#14856=CARTESIAN_POINT('',(-33.,72.,-131.665337888822));
#14857=CARTESIAN_POINT('Origin',(-33.0000000000006,67.9999999999993,-139.329431198144));
#14858=CARTESIAN_POINT('',(-33.,72.,-572.988200899477));
#14859=CARTESIAN_POINT('Origin',(-32.9999999999998,68.0000000000002,-565.447580013871));
#14860=CARTESIAN_POINT('',(-33.,72.,-746.));
#14861=CARTESIAN_POINT('Origin',(-82.,72.,-746.));
#14862=CARTESIAN_POINT('',(-33.5,72.,-131.665337888822));
#14863=CARTESIAN_POINT('',(-82.,72.,-131.665337888822));
#14864=CARTESIAN_POINT('',(-33.5,72.,-572.988200899477));
#14865=CARTESIAN_POINT('',(-82.,72.,-572.988200899477));
#14866=CARTESIAN_POINT('',(-33.5,72.,-746.));
#14867=CARTESIAN_POINT('',(-81.,72.,-746.));
#14868=CARTESIAN_POINT('',(-33.5,72.,-746.));
#14869=CARTESIAN_POINT('Origin',(-81.,68.,-746.));
#14870=CARTESIAN_POINT('',(-85.,68.,-746.));
#14871=CARTESIAN_POINT('Origin',(-85.,-1.00421037530083E-14,-746.));
#14872=CARTESIAN_POINT('',(-85.,0.99999999999999,-746.));
#14873=CARTESIAN_POINT('Origin',(-81.,0.99999999999999,-746.));
#14874=CARTESIAN_POINT('',(-81.,-3.00000000000001,-746.));
#14875=CARTESIAN_POINT('Origin',(3.67394039744206E-16,-3.,-746.));
#14876=CARTESIAN_POINT('',(3.67394039744206E-16,-3.,0.));
#14877=CARTESIAN_POINT('',(3.67394039744206E-16,-3.,0.));
#14878=CARTESIAN_POINT('',(3.67394039744206E-16,-3.,-746.));
#14879=CARTESIAN_POINT('Origin',(0.,0.,-746.));
#14880=CARTESIAN_POINT('',(0.,0.,0.));
#14881=CARTESIAN_POINT('',(0.,0.,0.));
#14882=CARTESIAN_POINT('',(0.,0.,-746.));
#14883=CARTESIAN_POINT('Origin',(0.,0.,-746.));
#14884=CARTESIAN_POINT('',(0.,0.,0.));
#14885=CARTESIAN_POINT('',(-81.,-9.91963907309357E-15,-746.));
#14886=CARTESIAN_POINT('Origin',(-81.,0.99999999999999,-746.));
#14887=CARTESIAN_POINT('',(-82.,0.99999999999999,-746.));
#14888=CARTESIAN_POINT('Origin',(-82.,-1.00421037530083E-14,-746.));
#14889=CARTESIAN_POINT('',(-82.,68.,-746.));
#14890=CARTESIAN_POINT('Origin',(-81.,68.,-746.));
#14891=CARTESIAN_POINT('',(-81.,69.,-746.));
#14892=CARTESIAN_POINT('Origin',(-82.,69.,-746.));
#14893=CARTESIAN_POINT('',(-33.5,69.,-137.413407870812));
#14894=CARTESIAN_POINT('',(-33.5,69.,-746.));
#14895=CARTESIAN_POINT('',(-33.5,69.,-567.332735235272));
#14896=CARTESIAN_POINT('',(-33.5,69.,-746.));
#14897=CARTESIAN_POINT('',(-33.,69.,-567.332735235272));
#14898=CARTESIAN_POINT('',(-82.,69.,-567.332735235272));
#14899=CARTESIAN_POINT('',(-33.,69.,-137.413407870813));
#14900=CARTESIAN_POINT('',(-33.,69.,-746.));
#14901=CARTESIAN_POINT('',(-82.,69.,-137.413407870813));
#14902=CARTESIAN_POINT('Origin',(-33.,68.,-746.));
#14903=CARTESIAN_POINT('Origin',(-32.9999999999994,68.0000000000007,-565.447580013872));
#14904=CARTESIAN_POINT('Origin',(-33.0000000000001,67.9999999999998,-139.329431198143));
#14905=CARTESIAN_POINT('Origin',(-33.,68.,0.));
#14906=CARTESIAN_POINT('Origin',(-33.5,0.,0.));
#14907=CARTESIAN_POINT('',(-33.5,72.6655742581807,-574.242911687517));
#14908=CARTESIAN_POINT('Origin',(-33.5,72.6655742581807,-574.242911687517));
#14909=CARTESIAN_POINT('Origin',(-33.5,50.,-173.817851090086));
#14910=CARTESIAN_POINT('',(-33.5,50.,-173.817851090086));
#14911=CARTESIAN_POINT('Origin',(-33.5,0.,0.));
#14912=CARTESIAN_POINT('',(0.,0.,0.));
#14913=CARTESIAN_POINT('Origin',(207.953766646564,-91.,12.8058966268102));
#14914=CARTESIAN_POINT('',(207.953766646564,-4.7625,6.45589662681021));
#14915=CARTESIAN_POINT('Origin',(207.953766646564,-4.7625,12.8058966268102));
#14916=CARTESIAN_POINT('',(207.953766646564,0.,6.45589662681021));
#14917=CARTESIAN_POINT('',(207.953766646564,-91.,6.45589662681021));
#14918=CARTESIAN_POINT('Origin',(207.953766646564,0.,12.8058966268102));
#14919=CARTESIAN_POINT('Origin',(207.953766646564,-91.,88.7941033731899));
#14920=CARTESIAN_POINT('',(207.953766646564,-4.7625,82.4441033731899));
#14921=CARTESIAN_POINT('Origin',(207.953766646564,-4.7625,88.7941033731899));
#14922=CARTESIAN_POINT('',(207.953766646564,0.,82.4441033731899));
#14923=CARTESIAN_POINT('',(207.953766646564,-91.,82.4441033731899));
#14924=CARTESIAN_POINT('Origin',(207.953766646564,0.,88.7941033731899));
#14925=CARTESIAN_POINT('Origin',(19.8411166279443,-91.,50.8000000000001));
#14926=CARTESIAN_POINT('',(19.8411166279443,-4.7625,44.4500000000001));
#14927=CARTESIAN_POINT('Origin',(19.8411166279443,-4.7625,50.8000000000001));
#14928=CARTESIAN_POINT('',(19.8411166279443,0.,44.4500000000001));
#14929=CARTESIAN_POINT('',(19.8411166279443,-91.,44.4500000000001));
#14930=CARTESIAN_POINT('Origin',(19.8411166279443,0.,50.8000000000001));
#14931=CARTESIAN_POINT('Origin',(225.2375,1.,101.6));
#14932=CARTESIAN_POINT('',(225.2375,1.,101.6));
#14933=CARTESIAN_POINT('',(230.,1.,101.6));
#14934=CARTESIAN_POINT('',(225.2375,1.,101.6));
#14935=CARTESIAN_POINT('',(224.2375,0.,101.6));
#14936=CARTESIAN_POINT('Origin',(224.2375,1.,101.6));
#14937=CARTESIAN_POINT('',(224.2375,-4.7625,101.6));
#14938=CARTESIAN_POINT('',(224.2375,-4.7625,101.6));
#14939=CARTESIAN_POINT('Origin',(224.2375,1.,101.6));
#14940=CARTESIAN_POINT('Origin',(224.2375,-4.7625,101.6));
#14941=CARTESIAN_POINT('',(225.2375,59.475,101.6));
#14942=CARTESIAN_POINT('',(225.2375,0.,101.6));
#14943=CARTESIAN_POINT('',(230.,59.475,101.6));
#14944=CARTESIAN_POINT('',(230.,0.,101.6));
#14945=CARTESIAN_POINT('',(230.,59.475,101.6));
#14946=CARTESIAN_POINT('Origin',(224.2375,0.,0.));
#14947=CARTESIAN_POINT('',(224.2375,0.,0.));
#14948=CARTESIAN_POINT('',(224.2375,-4.7625,0.));
#14949=CARTESIAN_POINT('',(224.2375,0.,0.));
#14950=CARTESIAN_POINT('',(225.2375,1.,0.));
#14951=CARTESIAN_POINT('Origin',(224.2375,1.,0.));
#14952=CARTESIAN_POINT('',(230.,1.,0.));
#14953=CARTESIAN_POINT('',(230.,1.,0.));
#14954=CARTESIAN_POINT('Origin',(224.2375,1.,0.));
#14955=CARTESIAN_POINT('Origin',(230.,1.,0.));
#14956=CARTESIAN_POINT('',(0.,0.,0.));
#14957=CARTESIAN_POINT('',(0.,0.,0.));
#14958=CARTESIAN_POINT('',(0.,-4.7625,0.));
#14959=CARTESIAN_POINT('',(0.,-4.7625,0.));
#14960=CARTESIAN_POINT('',(0.,-4.7625,0.));
#14961=CARTESIAN_POINT('Origin',(231.,65.2375,101.6));
#14962=CARTESIAN_POINT('',(231.,65.2375,101.6));
#14963=CARTESIAN_POINT('',(231.,60.475,101.6));
#14964=CARTESIAN_POINT('',(231.,65.2375,101.6));
#14965=CARTESIAN_POINT('Origin',(231.,59.475,101.6));
#14966=CARTESIAN_POINT('Origin',(231.,59.475,101.6));
#14967=CARTESIAN_POINT('Origin',(230.,59.475,101.6));
#14968=CARTESIAN_POINT('',(264.2375,65.2375,101.6));
#14969=CARTESIAN_POINT('',(225.2375,65.2375,101.6));
#14970=CARTESIAN_POINT('',(264.2375,60.475,101.6));
#14971=CARTESIAN_POINT('',(225.2375,60.475,101.6));
#14972=CARTESIAN_POINT('',(264.2375,60.475,101.6));
#14973=CARTESIAN_POINT('Origin',(225.2375,59.475,0.));
#14974=CARTESIAN_POINT('',(225.2375,59.475,0.));
#14975=CARTESIAN_POINT('',(230.,59.475,0.));
#14976=CARTESIAN_POINT('',(225.2375,59.475,0.));
#14977=CARTESIAN_POINT('',(231.,65.2375,0.));
#14978=CARTESIAN_POINT('Origin',(231.,59.475,0.));
#14979=CARTESIAN_POINT('',(231.,60.475,0.));
#14980=CARTESIAN_POINT('',(231.,60.475,0.));
#14981=CARTESIAN_POINT('Origin',(231.,59.475,0.));
#14982=CARTESIAN_POINT('Origin',(231.,60.475,0.));
#14983=CARTESIAN_POINT('',(225.2375,0.,0.));
#14984=CARTESIAN_POINT('',(230.,0.,0.));
#14985=CARTESIAN_POINT('Origin',(270.,59.475,101.6));
#14986=CARTESIAN_POINT('',(270.,59.475,101.6));
#14987=CARTESIAN_POINT('',(265.2375,59.475,101.6));
#14988=CARTESIAN_POINT('',(270.,59.475,101.6));
#14989=CARTESIAN_POINT('Origin',(264.2375,59.475,101.6));
#14990=CARTESIAN_POINT('Origin',(264.2375,59.475,101.6));
#14991=CARTESIAN_POINT('Origin',(264.2375,60.475,101.6));
#14992=CARTESIAN_POINT('',(270.,-3.54548993221453,101.6));
#14993=CARTESIAN_POINT('',(265.2375,-3.54548993221453,101.6));
#14994=CARTESIAN_POINT('',(356.2375,-3.54548993221453,101.6));
#14995=CARTESIAN_POINT('',(270.,65.2375,101.6));
#14996=CARTESIAN_POINT('',(265.2375,65.2375,101.6));
#14997=CARTESIAN_POINT('Origin',(264.2375,65.2375,0.));
#14998=CARTESIAN_POINT('',(264.2375,65.2375,0.));
#14999=CARTESIAN_POINT('',(264.2375,60.475,0.));
#15000=CARTESIAN_POINT('',(264.2375,65.2375,0.));
#15001=CARTESIAN_POINT('',(270.,59.475,0.));
#15002=CARTESIAN_POINT('Origin',(264.2375,59.475,0.));
#15003=CARTESIAN_POINT('',(265.2375,59.475,0.));
#15004=CARTESIAN_POINT('',(265.2375,59.475,0.));
#15005=CARTESIAN_POINT('Origin',(264.2375,59.475,0.));
#15006=CARTESIAN_POINT('Origin',(265.2375,59.475,0.));
#15007=CARTESIAN_POINT('',(225.2375,65.2375,0.));
#15008=CARTESIAN_POINT('',(225.2375,60.475,0.));
#15009=CARTESIAN_POINT('Origin',(271.,-9.525,0.));
#15010=CARTESIAN_POINT('',(270.,-3.54548993221453,0.));
#15011=CARTESIAN_POINT('',(265.2375,-3.54548993221453,0.));
#15012=CARTESIAN_POINT('',(356.2375,-3.54548993221453,0.));
#15013=CARTESIAN_POINT('',(265.2375,65.2375,0.));
#15014=CARTESIAN_POINT('',(270.,65.2375,0.));
#15015=CARTESIAN_POINT('Origin',(270.,-9.525,101.6));
#15016=CARTESIAN_POINT('',(297.294,-9.52500000000001,65.8));
#15017=CARTESIAN_POINT('',(297.294,-9.525,35.8));
#15018=CARTESIAN_POINT('',(297.294,-9.525,101.6));
#15019=CARTESIAN_POINT('',(271.,-9.52500000000001,65.8));
#15020=CARTESIAN_POINT('',(356.2375,-9.52500000000001,65.8));
#15021=CARTESIAN_POINT('',(271.,-9.525,35.8));
#15022=CARTESIAN_POINT('',(271.,-9.525,101.6));
#15023=CARTESIAN_POINT('',(356.2375,-9.525,35.8));
#15024=CARTESIAN_POINT('Origin',(297.294,-4.7625,101.6));
#15025=CARTESIAN_POINT('',(297.294,-4.7625,65.8));
#15026=CARTESIAN_POINT('',(297.294,-4.7625,65.8));
#15027=CARTESIAN_POINT('',(297.294,-4.7625,35.8));
#15028=CARTESIAN_POINT('',(297.294,-4.7625,35.8));
#15029=CARTESIAN_POINT('',(297.294,-4.7625,101.6));
#15030=CARTESIAN_POINT('Origin',(270.,-4.7625,101.6));
#15031=CARTESIAN_POINT('',(271.,-4.7625,65.8));
#15032=CARTESIAN_POINT('',(270.,-4.7625,65.8));
#15033=CARTESIAN_POINT('',(271.,-4.7625,35.8));
#15034=CARTESIAN_POINT('',(270.,-4.7625,35.8));
#15035=CARTESIAN_POINT('',(271.,-4.7625,101.6));
#15036=CARTESIAN_POINT('Origin',(271.,-3.7625,101.6));
#15037=CARTESIAN_POINT('',(270.,-3.7625,65.8));
#15038=CARTESIAN_POINT('Origin',(271.,-3.7625,65.8));
#15039=CARTESIAN_POINT('',(270.,-3.7625,35.8));
#15040=CARTESIAN_POINT('Origin',(271.,-3.7625,35.8));
#15041=CARTESIAN_POINT('',(270.,-3.7625,101.6));
#15042=CARTESIAN_POINT('Origin',(270.,65.2375,101.6));
#15043=CARTESIAN_POINT('',(270.,-3.54548993221453,65.8));
#15044=CARTESIAN_POINT('',(270.,65.2375,65.8));
#15045=CARTESIAN_POINT('',(270.,-3.54548993221453,35.8));
#15046=CARTESIAN_POINT('',(270.,65.2375,35.8));
#15047=CARTESIAN_POINT('',(270.,-3.54548993221453,101.6));
#15048=CARTESIAN_POINT('',(270.,59.475,101.6));
#15049=CARTESIAN_POINT('',(270.,-3.54548993221453,101.6));
#15050=CARTESIAN_POINT('Origin',(264.2375,59.475,101.6));
#15051=CARTESIAN_POINT('',(264.2375,65.2375,101.6));
#15052=CARTESIAN_POINT('Origin',(225.2375,65.2375,101.6));
#15053=CARTESIAN_POINT('',(231.,65.2375,101.6));
#15054=CARTESIAN_POINT('Origin',(231.,59.475,101.6));
#15055=CARTESIAN_POINT('',(225.2375,59.475,101.6));
#15056=CARTESIAN_POINT('Origin',(225.2375,0.,101.6));
#15057=CARTESIAN_POINT('',(225.2375,1.,101.6));
#15058=CARTESIAN_POINT('Origin',(224.2375,1.,101.6));
#15059=CARTESIAN_POINT('',(224.2375,0.,101.6));
#15060=CARTESIAN_POINT('Origin',(0.,0.,101.6));
#15061=CARTESIAN_POINT('',(0.,0.,101.6));
#15062=CARTESIAN_POINT('',(0.,0.,101.6));
#15063=CARTESIAN_POINT('',(0.,0.,101.6));
#15064=CARTESIAN_POINT('Origin',(0.,-4.7625,101.6));
#15065=CARTESIAN_POINT('',(0.,-4.7625,101.6));
#15066=CARTESIAN_POINT('',(0.,-4.7625,101.6));
#15067=CARTESIAN_POINT('',(0.,-4.7625,101.6));
#15068=CARTESIAN_POINT('Origin',(0.,-4.7625,101.6));
#15069=CARTESIAN_POINT('',(224.2375,-4.7625,101.6));
#15070=CARTESIAN_POINT('',(0.,-4.7625,101.6));
#15071=CARTESIAN_POINT('Origin',(224.2375,1.,101.6));
#15072=CARTESIAN_POINT('',(230.,1.,101.6));
#15073=CARTESIAN_POINT('Origin',(230.,0.,101.6));
#15074=CARTESIAN_POINT('',(230.,59.475,101.6));
#15075=CARTESIAN_POINT('Origin',(231.,59.475,101.6));
#15076=CARTESIAN_POINT('',(231.,60.475,101.6));
#15077=CARTESIAN_POINT('Origin',(225.2375,60.475,101.6));
#15078=CARTESIAN_POINT('',(264.2375,60.475,101.6));
#15079=CARTESIAN_POINT('Origin',(264.2375,59.475,101.6));
#15080=CARTESIAN_POINT('',(265.2375,59.475,101.6));
#15081=CARTESIAN_POINT('Origin',(265.2375,65.2375,101.6));
#15082=CARTESIAN_POINT('',(265.2375,-3.7625,65.8));
#15083=CARTESIAN_POINT('',(265.2375,-3.7625,35.8));
#15084=CARTESIAN_POINT('',(265.2375,-3.7625,101.6));
#15085=CARTESIAN_POINT('',(265.2375,-3.54548993221453,65.8));
#15086=CARTESIAN_POINT('',(265.2375,-9.52500000000001,65.8));
#15087=CARTESIAN_POINT('',(265.2375,-3.54548993221453,101.6));
#15088=CARTESIAN_POINT('',(265.2375,-3.54548993221453,35.8));
#15089=CARTESIAN_POINT('',(265.2375,-3.54548993221453,0.));
#15090=CARTESIAN_POINT('',(265.2375,-9.525,35.8));
#15091=CARTESIAN_POINT('Origin',(271.,-3.7625,101.6));
#15092=CARTESIAN_POINT('Origin',(271.,-3.7625,65.8));
#15093=CARTESIAN_POINT('Origin',(271.,-3.7625,35.8));
#15094=CARTESIAN_POINT('Origin',(271.,-3.7625,101.6));
#15095=CARTESIAN_POINT('Origin',(356.2375,-9.525,35.8));
#15096=CARTESIAN_POINT('',(356.2375,-3.54548993221453,35.8));
#15097=CARTESIAN_POINT('Origin',(356.2375,-3.54548993221453,0.));
#15098=CARTESIAN_POINT('Origin',(356.2375,-9.52500000000001,65.8));
#15099=CARTESIAN_POINT('',(356.2375,-3.54548993221453,65.8));
#15100=CARTESIAN_POINT('Origin',(356.2375,-3.54548993221453,101.6));
#15101=CARTESIAN_POINT('',(0.,0.,0.));
#15102=CARTESIAN_POINT('Origin',(37.3967602305982,34.,30.));
#15103=CARTESIAN_POINT('',(37.3967602305982,34.,30.));
#15104=CARTESIAN_POINT('',(37.3967602305982,31.,30.));
#15105=CARTESIAN_POINT('',(37.3967602305982,34.,30.));
#15106=CARTESIAN_POINT('',(34.6421882566514,32.9004022549204,30.));
#15107=CARTESIAN_POINT('Origin',(37.3967602305982,30.,30.));
#15108=CARTESIAN_POINT('',(36.7081172371115,30.7251005637301,30.));
#15109=CARTESIAN_POINT('',(36.7081172371115,30.7251005637301,30.));
#15110=CARTESIAN_POINT('Origin',(37.3967602305982,30.,30.));
#15111=CARTESIAN_POINT('Origin',(36.7081172371115,30.7251005637301,30.));
#15112=CARTESIAN_POINT('',(64.2032397694018,34.,30.));
#15113=CARTESIAN_POINT('',(35.8,34.,30.));
#15114=CARTESIAN_POINT('',(64.2032397694018,31.,30.));
#15115=CARTESIAN_POINT('',(35.8,31.,30.));
#15116=CARTESIAN_POINT('',(64.2032397694018,31.,30.));
#15117=CARTESIAN_POINT('Origin',(34.6421882566514,32.9004022549204,0.));
#15118=CARTESIAN_POINT('',(34.6421882566514,32.9004022549204,0.));
#15119=CARTESIAN_POINT('',(36.7081172371115,30.7251005637301,0.));
#15120=CARTESIAN_POINT('',(34.6421882566514,32.9004022549204,0.));
#15121=CARTESIAN_POINT('',(37.3967602305982,34.,0.));
#15122=CARTESIAN_POINT('Origin',(37.3967602305982,30.,0.));
#15123=CARTESIAN_POINT('',(37.3967602305982,31.,0.));
#15124=CARTESIAN_POINT('',(37.3967602305982,31.,0.));
#15125=CARTESIAN_POINT('Origin',(37.3967602305982,30.,0.));
#15126=CARTESIAN_POINT('Origin',(37.3967602305982,31.,0.));
#15127=CARTESIAN_POINT('',(0.,0.,0.));
#15128=CARTESIAN_POINT('',(0.,0.,0.));
#15129=CARTESIAN_POINT('',(2.06592898046005,-2.17530169119028,0.));
#15130=CARTESIAN_POINT('',(2.06592898046005,-2.17530169119028,0.));
#15131=CARTESIAN_POINT('',(2.06592898046005,-2.17530169119028,0.));
#15132=CARTESIAN_POINT('Origin',(66.9578117433485,32.9004022549204,30.));
#15133=CARTESIAN_POINT('',(66.9578117433485,32.9004022549204,30.));
#15134=CARTESIAN_POINT('',(64.8918827628885,30.7251005637301,30.));
#15135=CARTESIAN_POINT('',(66.9578117433485,32.9004022549204,30.));
#15136=CARTESIAN_POINT('Origin',(64.2032397694018,30.,30.));
#15137=CARTESIAN_POINT('Origin',(64.2032397694018,30.,30.));
#15138=CARTESIAN_POINT('Origin',(64.2032397694018,31.,30.));
#15139=CARTESIAN_POINT('',(101.6,0.,30.));
#15140=CARTESIAN_POINT('',(65.8,34.,30.));
#15141=CARTESIAN_POINT('',(99.53407101954,-2.17530169119028,30.));
#15142=CARTESIAN_POINT('',(63.73407101954,31.8246983088097,30.));
#15143=CARTESIAN_POINT('',(101.6,0.,30.));
#15144=CARTESIAN_POINT('Origin',(64.2032397694018,34.,0.));
#15145=CARTESIAN_POINT('',(64.2032397694018,34.,0.));
#15146=CARTESIAN_POINT('',(64.2032397694018,31.,0.));
#15147=CARTESIAN_POINT('',(64.2032397694018,34.,0.));
#15148=CARTESIAN_POINT('',(66.9578117433485,32.9004022549204,0.));
#15149=CARTESIAN_POINT('Origin',(64.2032397694018,30.,0.));
#15150=CARTESIAN_POINT('',(64.8918827628885,30.7251005637301,0.));
#15151=CARTESIAN_POINT('',(64.8918827628885,30.7251005637301,0.));
#15152=CARTESIAN_POINT('Origin',(64.2032397694018,30.,0.));
#15153=CARTESIAN_POINT('Origin',(64.8918827628885,30.7251005637301,0.));
#15154=CARTESIAN_POINT('',(35.8,34.,0.));
#15155=CARTESIAN_POINT('',(35.8,31.,0.));
#15156=CARTESIAN_POINT('Origin',(63.73407101954,31.8246983088097,30.));
#15157=CARTESIAN_POINT('',(99.53407101954,-2.17530169119028,0.));
#15158=CARTESIAN_POINT('',(63.73407101954,31.8246983088097,0.));
#15159=CARTESIAN_POINT('',(99.53407101954,-2.17530169119028,30.));
#15160=CARTESIAN_POINT('',(64.8918827628885,30.7251005637301,30.));
#15161=CARTESIAN_POINT('Origin',(101.6,0.,30.));
#15162=CARTESIAN_POINT('',(101.6,0.,0.));
#15163=CARTESIAN_POINT('',(101.6,0.,0.));
#15164=CARTESIAN_POINT('',(101.6,0.,30.));
#15165=CARTESIAN_POINT('Origin',(65.8,34.,30.));
#15166=CARTESIAN_POINT('',(65.8,34.,0.));
#15167=CARTESIAN_POINT('',(66.9578117433485,32.9004022549204,30.));
#15168=CARTESIAN_POINT('Origin',(64.2032397694018,30.,30.));
#15169=CARTESIAN_POINT('',(64.2032397694018,34.,30.));
#15170=CARTESIAN_POINT('Origin',(35.8,34.,30.));
#15171=CARTESIAN_POINT('',(37.3967602305982,34.,30.));
#15172=CARTESIAN_POINT('Origin',(37.3967602305982,30.,30.));
#15173=CARTESIAN_POINT('',(34.6421882566514,32.9004022549204,30.));
#15174=CARTESIAN_POINT('Origin',(0.,0.,30.));
#15175=CARTESIAN_POINT('',(0.,0.,30.));
#15176=CARTESIAN_POINT('',(0.,0.,30.));
#15177=CARTESIAN_POINT('',(0.,0.,30.));
#15178=CARTESIAN_POINT('Origin',(2.06592898046005,-2.17530169119028,30.));
#15179=CARTESIAN_POINT('',(2.06592898046005,-2.17530169119028,30.));
#15180=CARTESIAN_POINT('',(2.06592898046005,-2.17530169119028,30.));
#15181=CARTESIAN_POINT('',(2.06592898046005,-2.17530169119028,30.));
#15182=CARTESIAN_POINT('Origin',(2.06592898046005,-2.17530169119028,30.));
#15183=CARTESIAN_POINT('',(36.7081172371115,30.7251005637301,30.));
#15184=CARTESIAN_POINT('',(2.06592898046005,-2.17530169119028,30.));
#15185=CARTESIAN_POINT('Origin',(37.3967602305982,30.,30.));
#15186=CARTESIAN_POINT('',(37.3967602305982,31.,30.));
#15187=CARTESIAN_POINT('Origin',(35.8,31.,30.));
#15188=CARTESIAN_POINT('',(64.2032397694018,31.,30.));
#15189=CARTESIAN_POINT('Origin',(64.2032397694018,30.,30.));
#15190=CARTESIAN_POINT('Origin',(64.2032397694018,30.,30.));
#15191=CARTESIAN_POINT('Origin',(64.2032397694018,30.,0.));
#15192=CARTESIAN_POINT('',(0.,0.,0.));
#15193=CARTESIAN_POINT('',(0.,0.,0.));
#15194=CARTESIAN_POINT('',(0.,0.,0.));
#15195=CARTESIAN_POINT('Origin',(0.,-3.175,0.));
#15196=CARTESIAN_POINT('',(19.112550640874,0.,14.0969999999996));
#15197=CARTESIAN_POINT('',(19.1125506408747,0.,-14.0970000000004));
#15198=CARTESIAN_POINT('Origin',(0.,0.,0.));
#15199=CARTESIAN_POINT('',(20.6538081718591,-3.175,-17.272));
#15200=CARTESIAN_POINT('Ctrl Pts',(19.1125506408748,2.77555756154723E-15,
-14.0970000000003));
#15201=CARTESIAN_POINT('Ctrl Pts',(19.1138953037088,2.51110454471956E-15,
-14.0996626540109));
#15202=CARTESIAN_POINT('Ctrl Pts',(19.1152398533713,-3.34947705096863E-6,
-14.1023253649212));
#15203=CARTESIAN_POINT('Ctrl Pts',(19.2418153345357,-0.000634081878517632,
-14.3530185739992));
#15204=CARTESIAN_POINT('Ctrl Pts',(19.3659139541285,-0.0303225597182667,
-14.6012742217102));
#15205=CARTESIAN_POINT('Ctrl Pts',(19.6053472178254,-0.147431072287969,
-15.0846659662088));
#15206=CARTESIAN_POINT('Ctrl Pts',(19.7204852634609,-0.233951293638394,
-15.3193409130674));
#15207=CARTESIAN_POINT('Ctrl Pts',(20.0027307446042,-0.530651124933933,
-15.8991978108223));
#15208=CARTESIAN_POINT('Ctrl Pts',(20.1588027445859,-0.78198114677237,-16.22458960826));
#15209=CARTESIAN_POINT('Ctrl Pts',(20.4057082326115,-1.38098045537426,-16.7435774284381));
#15210=CARTESIAN_POINT('Ctrl Pts',(20.4990644060442,-1.71252771315431,-16.9419056998126));
#15211=CARTESIAN_POINT('Ctrl Pts',(20.6225575632283,-2.42708028688262,-17.2049905219328));
#15212=CARTESIAN_POINT('Ctrl Pts',(20.6538081718602,-2.79834314217251,-17.272));
#15213=CARTESIAN_POINT('Ctrl Pts',(20.6538081718602,-3.175,-17.272));
#15214=CARTESIAN_POINT('',(20.6538081718601,-3.175,17.272));
#15215=CARTESIAN_POINT('Origin',(0.,-3.175,0.));
#15216=CARTESIAN_POINT('Ctrl Pts',(20.6538081718602,-3.175,17.272));
#15217=CARTESIAN_POINT('Ctrl Pts',(20.6538081718602,-2.79834314217248,17.272));
#15218=CARTESIAN_POINT('Ctrl Pts',(20.6225575632284,-2.42708028688257,17.2049905219327));
#15219=CARTESIAN_POINT('Ctrl Pts',(20.4990644060443,-1.71252771315431,16.9419056998125));
#15220=CARTESIAN_POINT('Ctrl Pts',(20.4057082326115,-1.38098045537427,16.743577428438));
#15221=CARTESIAN_POINT('Ctrl Pts',(20.1588027445859,-0.781981146772372,
16.22458960826));
#15222=CARTESIAN_POINT('Ctrl Pts',(20.0027307446043,-0.530651124933935,
15.8991978108223));
#15223=CARTESIAN_POINT('Ctrl Pts',(19.720485263461,-0.233951293638397,15.3193409130673));
#15224=CARTESIAN_POINT('Ctrl Pts',(19.6053472178255,-0.147431072287971,
15.0846659662087));
#15225=CARTESIAN_POINT('Ctrl Pts',(19.3659139541288,-0.0303225597184072,
14.6012742217107));
#15226=CARTESIAN_POINT('Ctrl Pts',(19.2418153345369,-0.000634081878525383,
14.3530185740028));
#15227=CARTESIAN_POINT('Ctrl Pts',(19.1152398533712,-3.34947705052422E-6,
14.1023253649209));
#15228=CARTESIAN_POINT('Ctrl Pts',(19.1138953037088,2.77539452102732E-15,
14.0996626540107));
#15229=CARTESIAN_POINT('Ctrl Pts',(19.1125506408747,2.77555756156289E-15,
14.097));
#15230=CARTESIAN_POINT('Origin',(0.,-73.5076,0.));
#15231=CARTESIAN_POINT('',(20.6538081718591,-62.4429468166364,-17.272));
#15232=CARTESIAN_POINT('',(20.6538081718601,-62.4429468166364,17.272));
#15233=CARTESIAN_POINT('Origin',(-3.33553976368163E-12,-39.4709528472701,
-7.16759984698001E-12));
#15234=CARTESIAN_POINT('',(20.6538081718601,-73.5076,17.272));
#15235=CARTESIAN_POINT('',(20.6538081718591,-73.5076,-17.272));
#15236=CARTESIAN_POINT('',(8.56788885112247,-6.42480436244998,25.5243620220912));
#15237=CARTESIAN_POINT('',(8.22877293383428,-5.94049664112041,25.6356991713383));
#15238=CARTESIAN_POINT('Ctrl Pts',(8.56788885112333,-6.42480436245023,25.5243620220917));
#15239=CARTESIAN_POINT('Ctrl Pts',(8.58247740214554,-6.38472264793424,25.5194650110107));
#15240=CARTESIAN_POINT('Ctrl Pts',(8.5896525553061,-6.34189741119553,25.5170461648507));
#15241=CARTESIAN_POINT('Ctrl Pts',(8.5896525553061,-6.30137626259123,25.5170461648507));
#15242=CARTESIAN_POINT('Ctrl Pts',(8.5896525553061,-6.25616522228443,25.5170461648507));
#15243=CARTESIAN_POINT('Ctrl Pts',(8.58062470445952,-6.20812464852199,25.5200905073257));
#15244=CARTESIAN_POINT('Ctrl Pts',(8.54445711937874,-6.12016084404096,25.5322226285827));
#15245=CARTESIAN_POINT('Ctrl Pts',(8.51733361893661,-6.08022910834043,25.5412971267874));
#15246=CARTESIAN_POINT('Ctrl Pts',(8.45392015775191,-6.01552543072761,25.5623588354995));
#15247=CARTESIAN_POINT('Ctrl Pts',(8.41275363352234,-5.98712521613906,25.5759571610809));
#15248=CARTESIAN_POINT('Ctrl Pts',(8.32293675216143,-5.94961527321306,25.6053262471586));
#15249=CARTESIAN_POINT('Ctrl Pts',(8.27428764510786,-5.94049664112042,25.6210894576849));
#15250=CARTESIAN_POINT('Ctrl Pts',(8.22877293383528,-5.94049664112042,25.6356991713388));
#15251=CARTESIAN_POINT('',(7.73378213538389,-8.71649372935708,25.7893464415522));
#15252=CARTESIAN_POINT('Origin',(0.,-29.9648855133081,0.));
#15253=CARTESIAN_POINT('',(6.73442318361918,-8.71649372935708,26.0681668013675));
#15254=CARTESIAN_POINT('Origin',(0.,-8.71649372935708,0.));
#15255=CARTESIAN_POINT('',(7.46137038829266,-6.71922269938127,25.8694748290084));
#15256=CARTESIAN_POINT('Origin',(0.,-27.2191693594009,0.));
#15257=CARTESIAN_POINT('',(7.30485534954441,-6.49569605876775,25.9141055088192));
#15258=CARTESIAN_POINT('Ctrl Pts',(7.46137038829304,-6.7192226993814,25.8694748290085));
#15259=CARTESIAN_POINT('Ctrl Pts',(7.4681114091947,-6.70070189667008,25.8675305586252));
#15260=CARTESIAN_POINT('Ctrl Pts',(7.47141517483894,-6.6809394711055,25.8665755616237));
#15261=CARTESIAN_POINT('Ctrl Pts',(7.47141517483894,-6.66225588406187,25.8665755616237));
#15262=CARTESIAN_POINT('Ctrl Pts',(7.47141517483895,-6.64116251891734,25.8665755616237));
#15263=CARTESIAN_POINT('Ctrl Pts',(7.46715702599097,-6.61874367022959,25.8678068851424));
#15264=CARTESIAN_POINT('Ctrl Pts',(7.4500759422442,-6.57771046543781,25.8727310545972));
#15265=CARTESIAN_POINT('Ctrl Pts',(7.43724862430546,-6.55909799494505,25.8764244082017));
#15266=CARTESIAN_POINT('Ctrl Pts',(7.4076825128636,-6.5295318835032,25.8849040489688));
#15267=CARTESIAN_POINT('Ctrl Pts',(7.38885282910554,-6.51672798041859,25.8902895930057));
#15268=CARTESIAN_POINT('Ctrl Pts',(7.34782088229779,-6.49980798326307,25.9019641922557));
#15269=CARTESIAN_POINT('Ctrl Pts',(7.32561685929433,-6.49569605876774,25.9082531044018));
#15270=CARTESIAN_POINT('Ctrl Pts',(7.30485534954484,-6.49569605876774,25.9141055088194));
#15271=CARTESIAN_POINT('',(7.15967440139299,-6.49569605876775,25.9545918570495));
#15272=CARTESIAN_POINT('Origin',(0.,-6.49569605876775,0.));
#15273=CARTESIAN_POINT('',(7.00315936264441,-6.60528906874269,25.9972601429725));
#15274=CARTESIAN_POINT('Ctrl Pts',(7.15967440139342,-6.49569605876774,25.9545918570497));
#15275=CARTESIAN_POINT('Ctrl Pts',(7.13873385917985,-6.49569605876778,25.9603683864925));
#15276=CARTESIAN_POINT('Ctrl Pts',(7.11633593789488,-6.49987971983431,25.9665166564859));
#15277=CARTESIAN_POINT('Ctrl Pts',(7.07499859064891,-6.51709172816763,25.9778105462796));
#15278=CARTESIAN_POINT('Ctrl Pts',(7.05605751854869,-6.53011538741213,25.9829572849828));
#15279=CARTESIAN_POINT('Ctrl Pts',(7.02667707910246,-6.55991159180965,25.9909177929906));
#15280=CARTESIAN_POINT('Ctrl Pts',(7.01406386516926,-6.57843611979423,25.994321472472));
#15281=CARTESIAN_POINT('Ctrl Pts',(7.00479133675568,-6.60094760079372,25.9968205124719));
#15282=CARTESIAN_POINT('Ctrl Pts',(7.0039524234652,-6.60311015204649,25.9970465077174));
#15283=CARTESIAN_POINT('Ctrl Pts',(7.0031593626448,-6.60528906874281,25.9972601429728));
#15284=CARTESIAN_POINT('',(6.23474370773658,-8.71649372935708,26.1921695721989));
#15285=CARTESIAN_POINT('Origin',(0.,-25.8463112824522,0.));
#15286=CARTESIAN_POINT('',(5.23538475597085,-8.71649372935708,26.4100837268066));
#15287=CARTESIAN_POINT('Origin',(0.,-8.71649372935708,0.));
#15288=CARTESIAN_POINT('',(6.2457650664991,-5.94049664112042,26.1895436144674));
#15289=CARTESIAN_POINT('Origin',(0.,-23.1005951285458,0.));
#15290=CARTESIAN_POINT('',(7.24512401826451,-5.94049664112042,25.9308687467263));
#15291=CARTESIAN_POINT('Origin',(0.,-5.94049664112042,0.));
#15292=CARTESIAN_POINT('',(7.15869873231657,-6.17794816273245,25.9548609793986));
#15293=CARTESIAN_POINT('Origin',(-0.0182813399441084,-25.8965381600848,
-0.0658369455926877));
#15294=CARTESIAN_POINT('',(7.49781464960465,-5.94049664112042,25.8589356215635));
#15295=CARTESIAN_POINT('Ctrl Pts',(7.49781464960508,-5.94049664112042,25.8589356215635));
#15296=CARTESIAN_POINT('Ctrl Pts',(7.45247387271553,-5.94049664112047,25.8720822083435));
#15297=CARTESIAN_POINT('Ctrl Pts',(7.40394492992665,-5.9495543680279,25.8860106185536));
#15298=CARTESIAN_POINT('Ctrl Pts',(7.3143206017176,-5.98686059614414,25.9114773875266));
#15299=CARTESIAN_POINT('Ctrl Pts',(7.27323128486029,-6.01512003264301,25.9230210822716));
#15300=CARTESIAN_POINT('Ctrl Pts',(7.20958399265881,-6.07973287738587,25.9407925807556));
#15301=CARTESIAN_POINT('Ctrl Pts',(7.18229087179023,-6.1198433116144,25.9483492526816));
#15302=CARTESIAN_POINT('Ctrl Pts',(7.1622206624012,-6.16857637445337,25.9538894019733));
#15303=CARTESIAN_POINT('Ctrl Pts',(7.16041065237484,-6.17324470102962,25.9543888088888));
#15304=CARTESIAN_POINT('Ctrl Pts',(7.15869873231696,-6.17794816273256,25.9548609793989));
#15305=CARTESIAN_POINT('Origin',(0.,-5.94049664112042,0.));
#15306=CARTESIAN_POINT('',(5.62533193759163,-6.42480436245001,26.3297819320992));
#15307=CARTESIAN_POINT('',(5.28621602030355,-5.94049664112041,26.3999563671358));
#15308=CARTESIAN_POINT('Ctrl Pts',(5.62533193759256,-6.42480436245034,26.3297819320993));
#15309=CARTESIAN_POINT('Ctrl Pts',(5.63995959985971,-6.38461519067206,26.3266567464849));
#15310=CARTESIAN_POINT('Ctrl Pts',(5.64709564177536,-6.34180741087569,26.3251227311981));
#15311=CARTESIAN_POINT('Ctrl Pts',(5.64709564177536,-6.30137626259123,26.3251227311981));
#15312=CARTESIAN_POINT('Ctrl Pts',(5.64709564177536,-6.25610361383163,26.3251227311981));
#15313=CARTESIAN_POINT('Ctrl Pts',(5.63805040451663,-6.20788827030969,26.3270680669035));
#15314=CARTESIAN_POINT('Ctrl Pts',(5.60149128427088,-6.11936267215691,26.3348708133353));
#15315=CARTESIAN_POINT('Ctrl Pts',(5.57398381597246,-6.07904902518731,26.3407197880059));
#15316=CARTESIAN_POINT('Ctrl Pts',(5.51018866497027,-6.01472493377371,26.354139780634));
#15317=CARTESIAN_POINT('Ctrl Pts',(5.46937520528438,-5.98669554819188,26.3626589704958));
#15318=CARTESIAN_POINT('Ctrl Pts',(5.38009343342981,-5.94958332553687,26.381024388344));
#15319=CARTESIAN_POINT('Ctrl Pts',(5.33162531866527,-5.94049664112042,26.3908638005752));
#15320=CARTESIAN_POINT('Ctrl Pts',(5.28621602030455,-5.94049664112042,26.3999563671358));
#15321=CARTESIAN_POINT('',(4.87765050780198,-8.47904220774524,26.4784875233413));
#15322=CARTESIAN_POINT('Origin',(0.,-21.8802768379213,0.));
#15323=CARTESIAN_POINT('',(4.53853459051412,-8.71649372935708,26.5387166187573));
#15324=CARTESIAN_POINT('Ctrl Pts',(4.53853459051412,-8.71649372935709,26.5387166187573));
#15325=CARTESIAN_POINT('Ctrl Pts',(4.58392376811759,-8.71649372935709,26.5309543612395));
#15326=CARTESIAN_POINT('Ctrl Pts',(4.63235861885573,-8.7074132610015,26.5225390940241));
#15327=CARTESIAN_POINT('Ctrl Pts',(4.72154377441757,-8.67037311230097,26.5068076303805));
#15328=CARTESIAN_POINT('Ctrl Pts',(4.76229410517978,-8.6424106466535,26.4994981399101));
#15329=CARTESIAN_POINT('Ctrl Pts',(4.82616017148578,-8.57815268809235,26.4879404552818));
#15330=CARTESIAN_POINT('Ctrl Pts',(4.8537364828052,-8.53777047295051,26.4828881532753));
#15331=CARTESIAN_POINT('Ctrl Pts',(4.87402021006453,-8.48869331088556,26.4791560854992));
#15332=CARTESIAN_POINT('Ctrl Pts',(4.87588759973028,-8.4838857578648,26.4788122718543));
#15333=CARTESIAN_POINT('Ctrl Pts',(4.87765050780197,-8.47904220774523,26.4784875233413));
#15334=CARTESIAN_POINT('',(2.80821735451831,-8.71649372935709,26.7771486773662));
#15335=CARTESIAN_POINT('Origin',(0.,-8.71649372935708,0.));
#15336=CARTESIAN_POINT('',(2.46910143723023,-8.23218600802769,26.8105448302094));
#15337=CARTESIAN_POINT('Ctrl Pts',(2.80821735451831,-8.71649372935709,26.7771486773663));
#15338=CARTESIAN_POINT('Ctrl Pts',(2.76297201682474,-8.71649372935709,26.7818937211368));
#15339=CARTESIAN_POINT('Ctrl Pts',(2.71467509600979,-8.70746524308079,26.7868309335259));
#15340=CARTESIAN_POINT('Ctrl Pts',(2.62575485223533,-8.67066459721526,26.7956933814771));
#15341=CARTESIAN_POINT('Ctrl Pts',(2.5851329492046,-8.64289055764062,26.7996250558906));
#15342=CARTESIAN_POINT('Ctrl Pts',(2.52103887724451,-8.57879648568053,26.8057302109898));
#15343=CARTESIAN_POINT('Ctrl Pts',(2.49326252312878,-8.53824343692207,26.8083151351361));
#15344=CARTESIAN_POINT('Ctrl Pts',(2.4564114193914,-8.44932964492528,26.8117168665583));
#15345=CARTESIAN_POINT('Ctrl Pts',(2.44733773304761,-8.40096871226767,26.8125402381125));
#15346=CARTESIAN_POINT('Ctrl Pts',(2.44733773304761,-8.31523356163696,26.8125402381125));
#15347=CARTESIAN_POINT('Ctrl Pts',(2.45445194905183,-8.27243514600453,26.8118939662506));
#15348=CARTESIAN_POINT('Ctrl Pts',(2.46910143723027,-8.23218600802771,26.8105448302094));
#15349=CARTESIAN_POINT('',(3.21678286702076,-6.17794816273248,26.7311444571013));
#15350=CARTESIAN_POINT('Origin',(0.0278753939838294,-14.939399423083,-199.839316375535));
#15351=CARTESIAN_POINT('',(3.55589878430884,-5.94049664112042,26.6881501763563));
#15352=CARTESIAN_POINT('Ctrl Pts',(3.55589878430884,-5.94049664112043,26.6881501763564));
#15353=CARTESIAN_POINT('Ctrl Pts',(3.51068916740624,-5.94049664112043,26.6941738543079));
#15354=CARTESIAN_POINT('Ctrl Pts',(3.46241339887269,-5.94951031598463,26.700477123615));
#15355=CARTESIAN_POINT('Ctrl Pts',(3.37349109889783,-5.98629437148475,26.7118577223488));
#15356=CARTESIAN_POINT('Ctrl Pts',(3.33284656792511,-6.01406762390689,26.7169413991736));
#15357=CARTESIAN_POINT('Ctrl Pts',(3.26874910998512,-6.07816508184689,26.7248590807041));
#15358=CARTESIAN_POINT('Ctrl Pts',(3.24097107076634,-6.11869944878777,26.7282290328136));
#15359=CARTESIAN_POINT('Ctrl Pts',(3.22051144018494,-6.16804423236154,26.7306955807504));
#15360=CARTESIAN_POINT('Ctrl Pts',(3.21859202879973,-6.17297753159653,26.7309267454874));
#15361=CARTESIAN_POINT('Ctrl Pts',(3.21678286702074,-6.17794816273246,26.7311444571018));
#15362=CARTESIAN_POINT('Origin',(0.,-5.94049664112045,0.));
#15363=CARTESIAN_POINT('',(-1.09388860520765,-8.71649372935708,26.9017691559383));
#15364=CARTESIAN_POINT('',(0.219605798478462,-5.10769751464934,26.9231043769711));
#15365=CARTESIAN_POINT('Origin',(0.,-5.71105948715027,0.));
#15366=CARTESIAN_POINT('',(-2.09324755697293,-8.71649372935708,26.8425052978519));
#15367=CARTESIAN_POINT('Origin',(0.,-8.71649372935708,0.));
#15368=CARTESIAN_POINT('',(-0.779753153286711,-5.10769751464934,26.9127063117023));
#15369=CARTESIAN_POINT('Origin',(0.,-2.96534333324559,0.));
#15370=CARTESIAN_POINT('Origin',(0.,-5.10769751464934,0.));
#15371=CARTESIAN_POINT('',(-5.78088092123807,-6.71922269938132,26.2960679907563));
#15372=CARTESIAN_POINT('',(-5.93739595998644,-6.49569605876778,26.2611710556546));
#15373=CARTESIAN_POINT('Ctrl Pts',(-5.78088092123727,-6.71922269938161,
26.2960679907562));
#15374=CARTESIAN_POINT('Ctrl Pts',(-5.77413056624824,-6.70067625147608,
26.2975519768176));
#15375=CARTESIAN_POINT('Ctrl Pts',(-5.7708361346913,-6.68091763595328,26.2982742077601));
#15376=CARTESIAN_POINT('Ctrl Pts',(-5.7708361346913,-6.6622558840619,26.2982742077601));
#15377=CARTESIAN_POINT('Ctrl Pts',(-5.7708361346913,-6.6412361011532,26.2982742077601));
#15378=CARTESIAN_POINT('Ctrl Pts',(-5.77506230185251,-6.61886114087643,
26.2973481406241));
#15379=CARTESIAN_POINT('Ctrl Pts',(-5.79211091061369,-6.57782483589241,
26.2935979387832));
#15380=CARTESIAN_POINT('Ctrl Pts',(-5.80493598083167,-6.55916469933821,
26.2907725344501));
#15381=CARTESIAN_POINT('Ctrl Pts',(-5.83451735873657,-6.5295833214333,26.284223709044));
#15382=CARTESIAN_POINT('Ctrl Pts',(-5.85332063645495,-6.51677115872571,
26.2800469204155));
#15383=CARTESIAN_POINT('Ctrl Pts',(-5.89435985810223,-6.4998260307421,26.2708722651223));
#15384=CARTESIAN_POINT('Ctrl Pts',(-5.91659684460641,-6.49569605876776,
26.2658735338251));
#15385=CARTESIAN_POINT('Ctrl Pts',(-5.93739595998544,-6.49569605876776,
26.2611710556546));
#15386=CARTESIAN_POINT('',(-6.0825769081374,-6.49569605876778,26.2279247016725));
#15387=CARTESIAN_POINT('Origin',(0.,-6.49569605876778,0.));
#15388=CARTESIAN_POINT('',(-6.23909194688599,-6.60528906874266,26.1911341426505));
#15389=CARTESIAN_POINT('Ctrl Pts',(-6.08257690813685,-6.49569605876778,
26.2279247016725));
#15390=CARTESIAN_POINT('Ctrl Pts',(-6.1033864468263,-6.49569605876784,26.2230987148305));
#15391=CARTESIAN_POINT('Ctrl Pts',(-6.12562302214156,-6.49982925402997,
26.2179128142556));
#15392=CARTESIAN_POINT('Ctrl Pts',(-6.1666564550697,-6.51677381265563,26.2082921742541));
#15393=CARTESIAN_POINT('Ctrl Pts',(-6.18545455328693,-6.52958236533443,
26.2038577760556));
#15394=CARTESIAN_POINT('Ctrl Pts',(-6.21502344136832,-6.55915125341583,
26.1968602491631));
#15395=CARTESIAN_POINT('Ctrl Pts',(-6.22784834643964,-6.57780069084445,
26.1938112329571));
#15396=CARTESIAN_POINT('Ctrl Pts',(-6.23733292310808,-6.60062066301478,
26.1915531548287));
#15397=CARTESIAN_POINT('Ctrl Pts',(-6.23823897926493,-6.60294555946596,
26.1913373313853));
#15398=CARTESIAN_POINT('Ctrl Pts',(-6.23909194688544,-6.60528906874285,
26.1911341426504));
#15399=CARTESIAN_POINT('',(-6.72407449593913,-7.937767671096,26.0708380796063));
#15400=CARTESIAN_POINT('Origin',(-0.331612293475181,9.62537809675131,-185.824370072778));
#15401=CARTESIAN_POINT('',(-6.56755945719079,-8.16129431170977,26.1107054438645));
#15402=CARTESIAN_POINT('Ctrl Pts',(-6.72407449593875,-7.93776767109617,
26.0708380796066));
#15403=CARTESIAN_POINT('Ctrl Pts',(-6.73082001522399,-7.95630083301493,
26.0690983053021));
#15404=CARTESIAN_POINT('Ctrl Pts',(-6.73411928248454,-7.97606120203618,
26.0682453089821));
#15405=CARTESIAN_POINT('Ctrl Pts',(-6.73411928248454,-8.01561678849232,
26.0682453089822));
#15406=CARTESIAN_POINT('Ctrl Pts',(-6.72994648429115,-8.0378404502637,26.0693245633319));
#15407=CARTESIAN_POINT('Ctrl Pts',(-6.71313981884611,-8.07861194698775,
26.0736570957254));
#15408=CARTESIAN_POINT('Ctrl Pts',(-6.70050261293776,-8.09715838855526,
26.0769105342835));
#15409=CARTESIAN_POINT('Ctrl Pts',(-6.67111249628907,-8.12691401591447,
26.0844450236741));
#15410=CARTESIAN_POINT('Ctrl Pts',(-6.65221072472771,-8.13991012637671,
26.0892762073244));
#15411=CARTESIAN_POINT('Ctrl Pts',(-6.61091557605922,-8.15710203255545,
26.0997703923063));
#15412=CARTESIAN_POINT('Ctrl Pts',(-6.58852066653471,-8.16129431170977,
26.1054331240893));
#15413=CARTESIAN_POINT('Ctrl Pts',(-6.56755945719023,-8.16129431170977,
26.1107054438648));
#15414=CARTESIAN_POINT('',(-6.42237850903926,-8.16129431170975,26.1467938815955));
#15415=CARTESIAN_POINT('Origin',(0.,-8.16129431170914,0.));
#15416=CARTESIAN_POINT('',(-6.26586347029112,-8.05170130173512,26.1847423315884));
#15417=CARTESIAN_POINT('Ctrl Pts',(-6.42237850903871,-8.16129431170975,
26.1467938815955));
#15418=CARTESIAN_POINT('Ctrl Pts',(-6.40144475589619,-8.16129431170982,
26.1519357925657));
#15419=CARTESIAN_POINT('Ctrl Pts',(-6.37906538869629,-8.15711193639077,
26.1574031826718));
#15420=CARTESIAN_POINT('Ctrl Pts',(-6.33778846604781,-8.13994358242459,
26.1674353960545));
#15421=CARTESIAN_POINT('Ctrl Pts',(-6.31888960835918,-8.1269613033143,26.1720011920392));
#15422=CARTESIAN_POINT('Ctrl Pts',(-6.28946945495755,-8.09720993119882,
26.1790865326894));
#15423=CARTESIAN_POINT('Ctrl Pts',(-6.27681432553571,-8.07864347657602,
26.1821206566255));
#15424=CARTESIAN_POINT('Ctrl Pts',(-6.26751058244999,-8.05608193744371,
26.184348178312));
#15425=CARTESIAN_POINT('Ctrl Pts',(-6.26666367414443,-8.0538998437546,26.1845508472487));
#15426=CARTESIAN_POINT('Ctrl Pts',(-6.26586347029062,-8.05170130173531,
26.1847423315884));
#15427=CARTESIAN_POINT('',(-6.10367600169992,-7.60609489406241,26.2230226188034));
#15428=CARTESIAN_POINT('Origin',(-0.000654570580991276,9.16181893640906,
0.00276694393421817));
#15429=CARTESIAN_POINT('',(-5.10431704993508,-7.60609489406241,26.4357281619734));
#15430=CARTESIAN_POINT('Origin',(0.,-7.60609489406241,0.));
#15431=CARTESIAN_POINT('',(-5.42204388819834,-8.47904220774522,26.3723949628103));
#15432=CARTESIAN_POINT('Origin',(-0.177565559653503,5.93004453829832,-191.69942270391));
#15433=CARTESIAN_POINT('',(-5.76115980548619,-8.71649372935708,26.3003956946595));
#15434=CARTESIAN_POINT('Ctrl Pts',(-5.76115980548519,-8.7164937293571,26.3003956946595));
#15435=CARTESIAN_POINT('Ctrl Pts',(-5.71584265024373,-8.71649372935721,
26.3103225176741));
#15436=CARTESIAN_POINT('Ctrl Pts',(-5.66740036000291,-8.70744089282411,
26.320798522175));
#15437=CARTESIAN_POINT('Ctrl Pts',(-5.57807573135901,-8.67034119955738,
26.3398734397227));
#15438=CARTESIAN_POINT('Ctrl Pts',(-5.53719751631319,-8.64228748072347,
26.3484783140346));
#15439=CARTESIAN_POINT('Ctrl Pts',(-5.47336108618307,-8.57789883127215,
26.3618119898267));
#15440=CARTESIAN_POINT('Ctrl Pts',(-5.44586150915486,-8.53758569389779,
26.3674935558645));
#15441=CARTESIAN_POINT('Ctrl Pts',(-5.42564056778768,-8.48860672087298,
26.3716553213831));
#15442=CARTESIAN_POINT('Ctrl Pts',(-5.42379097335401,-8.48384228476306,
26.3720357700859));
#15443=CARTESIAN_POINT('Ctrl Pts',(-5.42204388819745,-8.47904220774554,
26.3723949628103));
#15444=CARTESIAN_POINT('',(-7.49147704148144,-8.71649372935707,25.8607723731706));
#15445=CARTESIAN_POINT('Origin',(0.,-8.71649372935708,0.));
#15446=CARTESIAN_POINT('',(-7.83059295876941,-8.23218600802769,25.7601162635973));
#15447=CARTESIAN_POINT('Ctrl Pts',(-7.49147704148101,-8.71649372935708,
25.860772373171));
#15448=CARTESIAN_POINT('Ctrl Pts',(-7.53646889504271,-8.71649372935708,
25.8477389094698));
#15449=CARTESIAN_POINT('Ctrl Pts',(-7.58456980567226,-8.70757883468378,
25.8336645662906));
#15450=CARTESIAN_POINT('Ctrl Pts',(-7.67346512072657,-8.6709326300511,25.8073992703965));
#15451=CARTESIAN_POINT('Ctrl Pts',(-7.71425842539506,-8.64319357904026,
25.7952153971673));
#15452=CARTESIAN_POINT('Ctrl Pts',(-7.7782961463305,-8.57915585810482,25.7759767305356));
#15453=CARTESIAN_POINT('Ctrl Pts',(-7.80608255577103,-8.53885176365304,
25.7675615008496));
#15454=CARTESIAN_POINT('Ctrl Pts',(-7.84311941619419,-8.44995554926159,
25.7563123989324));
#15455=CARTESIAN_POINT('Ctrl Pts',(-7.8523566629517,-8.40135641909417,25.7534904593105));
#15456=CARTESIAN_POINT('Ctrl Pts',(-7.85235666295169,-8.31512015350478,
25.7534904593105));
#15457=CARTESIAN_POINT('Ctrl Pts',(-7.84519325028322,-8.27229997928044,
25.7556780483834));
#15458=CARTESIAN_POINT('Ctrl Pts',(-7.83059295876909,-8.23218600802787,
25.7601162635978));
#15459=CARTESIAN_POINT('',(-7.08291152897898,-6.17794816273248,25.9756451367942));
#15460=CARTESIAN_POINT('Origin',(0.,13.2821913271337,0.));
#15461=CARTESIAN_POINT('',(-6.74379561169079,-5.94049664112042,26.0657437405444));
#15462=CARTESIAN_POINT('Ctrl Pts',(-6.74379561169036,-5.94049664112043,
26.0657437405447));
#15463=CARTESIAN_POINT('Ctrl Pts',(-6.78925150951685,-5.94049664112049,
26.0539832748799));
#15464=CARTESIAN_POINT('Ctrl Pts',(-6.83779894684191,-5.9495975507762,26.0412830876675));
#15465=CARTESIAN_POINT('Ctrl Pts',(-6.92731394253395,-5.98688316074841,
26.0176140495437));
#15466=CARTESIAN_POINT('Ctrl Pts',(-6.96828078325991,-6.01507410506063,
26.0066523216136));
#15467=CARTESIAN_POINT('Ctrl Pts',(-7.03190769832015,-6.07956104289738,
25.9895189602093));
#15468=CARTESIAN_POINT('Ctrl Pts',(-7.05924850731276,-6.11970886266071,
25.982092720278));
#15469=CARTESIAN_POINT('Ctrl Pts',(-7.07936353182313,-6.16850915201986,
25.9766124032064));
#15470=CARTESIAN_POINT('Ctrl Pts',(-7.08118730524561,-6.17321089696031,
25.976115289666));
#15471=CARTESIAN_POINT('Ctrl Pts',(-7.08291152897855,-6.17794816273265,
25.9756451367942));
#15472=CARTESIAN_POINT('',(-5.01347837569566,-5.94049664112041,26.4531058776931));
#15473=CARTESIAN_POINT('Origin',(0.,-5.94049664112037,0.));
#15474=CARTESIAN_POINT('',(-4.6743624584068,-6.42480436244975,26.5151298621643));
#15475=CARTESIAN_POINT('Ctrl Pts',(-4.67436245840667,-6.4248043624498,26.5151298621643));
#15476=CARTESIAN_POINT('Ctrl Pts',(-4.6597265653962,-6.38459257688998,26.5177100293816));
#15477=CARTESIAN_POINT('Ctrl Pts',(-4.65259875422399,-6.34178678345437,
26.5189573858437));
#15478=CARTESIAN_POINT('Ctrl Pts',(-4.65259875422399,-6.30137626259108,
26.5189573858437));
#15479=CARTESIAN_POINT('Ctrl Pts',(-4.65259875422399,-6.25591339171108,
26.5189573858437));
#15480=CARTESIAN_POINT('Ctrl Pts',(-4.66171857209701,-6.2074825970309,26.5173623703316));
#15481=CARTESIAN_POINT('Ctrl Pts',(-4.69862468788111,-6.11856998626509,
26.5108478394745));
#15482=CARTESIAN_POINT('Ctrl Pts',(-4.7264068643022,-6.07808691891565,26.5059220549762));
#15483=CARTESIAN_POINT('Ctrl Pts',(-4.79051080155461,-6.01398298166325,
26.4944117387668));
#15484=CARTESIAN_POINT('Ctrl Pts',(-4.83121347567045,-5.98621274541281,
26.48703827067));
#15485=CARTESIAN_POINT('Ctrl Pts',(-4.92013971779749,-5.94947225422765,
26.4706638593908));
#15486=CARTESIAN_POINT('Ctrl Pts',(-4.96835995786548,-5.94049664112042,
26.4616568664949));
#15487=CARTESIAN_POINT('Ctrl Pts',(-5.01347837569466,-5.94049664112042,
26.4531058776931));
#15488=CARTESIAN_POINT('',(-4.90224098782865,-7.05089547641508,26.4739458580933));
#15489=CARTESIAN_POINT('Origin',(-0.133716749099482,6.05051743799337,-193.672571874459));
#15490=CARTESIAN_POINT('',(-5.90159993959483,-7.05089547641508,26.2692385529728));
#15491=CARTESIAN_POINT('Origin',(0.,-7.05089547641508,0.));
#15492=CARTESIAN_POINT('Origin',(0.00150046491639411,9.16774038864687,-0.00676982652117797));
#15493=CARTESIAN_POINT('',(-1.73180554487584,-6.42480436245001,26.868245673187));
#15494=CARTESIAN_POINT('',(-2.07092146216392,-5.94049664112041,26.8442370034525));
#15495=CARTESIAN_POINT('Ctrl Pts',(-1.7318055448758,-6.42480436245003,26.8682456731871));
#15496=CARTESIAN_POINT('Ctrl Pts',(-1.71715342939276,-6.38454800601317,
26.8691900822545));
#15497=CARTESIAN_POINT('Ctrl Pts',(-1.7100418406931,-6.34175109702807,26.8696396124525));
#15498=CARTESIAN_POINT('Ctrl Pts',(-1.7100418406931,-6.30137626259123,26.8696396124525));
#15499=CARTESIAN_POINT('Ctrl Pts',(-1.7100418406931,-6.25607168456321,26.8696396124525));
#15500=CARTESIAN_POINT('Ctrl Pts',(-1.71909504497057,-6.20775349047707,
26.8690682410886));
#15501=CARTESIAN_POINT('Ctrl Pts',(-1.75589191343006,-6.11888397629865,
26.8666886591259));
#15502=CARTESIAN_POINT('Ctrl Pts',(-1.78363507519411,-6.07833262371318,
26.864873897393));
#15503=CARTESIAN_POINT('Ctrl Pts',(-1.84769506340573,-6.01421100519085,
26.8605441599219));
#15504=CARTESIAN_POINT('Ctrl Pts',(-1.88831468380421,-5.98640475358986,
26.8577369204304));
#15505=CARTESIAN_POINT('Ctrl Pts',(-1.9772772131259,-5.94954812054788,26.8513340386393));
#15506=CARTESIAN_POINT('Ctrl Pts',(-2.0256191984005,-5.94049664112042,26.8477318850657));
#15507=CARTESIAN_POINT('Ctrl Pts',(-2.07092146216392,-5.94049664112042,
26.8442370034529));
#15508=CARTESIAN_POINT('',(-2.47948697466649,-8.47904220774524,26.8095863515728));
#15509=CARTESIAN_POINT('Origin',(-0.0112854406951732,-1.69771422001854,
-201.367417688525));
#15510=CARTESIAN_POINT('',(-2.81860289195435,-8.71649372935708,26.7760574718808));
#15511=CARTESIAN_POINT('Ctrl Pts',(-2.81860289195435,-8.71649372935709,
26.7760574718809));
#15512=CARTESIAN_POINT('Ctrl Pts',(-2.77330125802283,-8.71649372935709,
26.780826184248));
#15513=CARTESIAN_POINT('Ctrl Pts',(-2.72494783882919,-8.70744294587161,
26.7857879418825));
#15514=CARTESIAN_POINT('Ctrl Pts',(-2.63594075660522,-8.67055750696939,
26.7946933686408));
#15515=CARTESIAN_POINT('Ctrl Pts',(-2.59528852432374,-8.64272096090093,
26.7986435054389));
#15516=CARTESIAN_POINT('Ctrl Pts',(-2.53125456106965,-8.57856615084576,
26.8047673937377));
#15517=CARTESIAN_POINT('Ctrl Pts',(-2.50354065467085,-8.53804322801846,
26.8073572183543));
#15518=CARTESIAN_POINT('Ctrl Pts',(-2.48316201365914,-8.48880849578354,
26.8092462861295));
#15519=CARTESIAN_POINT('Ctrl Pts',(-2.48127087227637,-8.48394342614699,
26.8094213676443));
#15520=CARTESIAN_POINT('Ctrl Pts',(-2.4794869746665,-8.47904220774525,26.8095863515732));
#15521=CARTESIAN_POINT('',(-4.54892012795016,-8.71649372935708,26.5369384381381));
#15522=CARTESIAN_POINT('Origin',(0.,-8.71649372935708,0.));
#15523=CARTESIAN_POINT('',(-4.88803604523824,-8.23218600802767,26.4765722785343));
#15524=CARTESIAN_POINT('Ctrl Pts',(-4.54892012795016,-8.71649372935709,
26.5369384381381));
#15525=CARTESIAN_POINT('Ctrl Pts',(-4.5941252754373,-8.71649372935709,26.529189443062));
#15526=CARTESIAN_POINT('Ctrl Pts',(-4.64237613578329,-8.7074861731848,26.5207872721073));
#15527=CARTESIAN_POINT('Ctrl Pts',(-4.73127991399183,-8.67072184184772,
26.5050712901122));
#15528=CARTESIAN_POINT('Ctrl Pts',(-4.77193283717809,-8.64296225372639,
26.4977640903463));
#15529=CARTESIAN_POINT('Ctrl Pts',(-4.83599219322129,-8.57890289768319,
26.4861474365404));
#15530=CARTESIAN_POINT('Ctrl Pts',(-4.86377100641505,-8.53842462562448,
26.4810471788912));
#15531=CARTESIAN_POINT('Ctrl Pts',(-4.90067716865808,-8.44951695604782,
26.4742420360334));
#15532=CARTESIAN_POINT('Ctrl Pts',(-4.90979974942086,-8.4010849733851,26.4725450688178));
#15533=CARTESIAN_POINT('Ctrl Pts',(-4.90979974942086,-8.3151985155725,26.4725450688178));
#15534=CARTESIAN_POINT('Ctrl Pts',(-4.90267053689182,-8.27239394339123,
26.473870496674));
#15535=CARTESIAN_POINT('Ctrl Pts',(-4.88803604523819,-8.23218600802769,
26.4765722785343));
#15536=CARTESIAN_POINT('',(-4.14035461544759,-6.17794816273246,26.6037448427537));
#15537=CARTESIAN_POINT('Origin',(-0.111891229144148,4.89016404367311,-194.718276624975));
#15538=CARTESIAN_POINT('',(-3.8012386981594,-5.94049664112043,26.6543122282231));
#15539=CARTESIAN_POINT('Ctrl Pts',(-3.8012386981594,-5.94049664112043,26.6543122282233));
#15540=CARTESIAN_POINT('Ctrl Pts',(-3.84661033786681,-5.94049664112043,
26.6478416642419));
#15541=CARTESIAN_POINT('Ctrl Pts',(-3.89501713208822,-5.94957163919945,
26.6408079058698));
#15542=CARTESIAN_POINT('Ctrl Pts',(-3.98412178667441,-5.98655144861116,
26.6276280942498));
#15543=CARTESIAN_POINT('Ctrl Pts',(-4.02481984687951,-6.01445814023913,
26.6214886686791));
#15544=CARTESIAN_POINT('Ctrl Pts',(-4.08874583850554,-6.07866172201334,
26.6117448984678));
#15545=CARTESIAN_POINT('Ctrl Pts',(-4.11637951208125,-6.11910113170568,
26.6074715134895));
#15546=CARTESIAN_POINT('Ctrl Pts',(-4.13670432719905,-6.16824558655295,
26.6043127580451));
#15547=CARTESIAN_POINT('Ctrl Pts',(-4.1385823206751,-6.1730788228646,26.6040206659088));
#15548=CARTESIAN_POINT('Ctrl Pts',(-4.14035461544753,-6.17794816273248,
26.6037448427537));
#15549=CARTESIAN_POINT('Origin',(0.,-5.9404966411204,0.));
#15550=CARTESIAN_POINT('',(-3.33066907387547E-13,-6.93137777777542,26.924));
#15551=CARTESIAN_POINT('',(0.288891181294382,-7.4121734434362,26.9224500721121));
#15552=CARTESIAN_POINT('Ctrl Pts',(0.28889118129438,-7.41217344343621,26.9224500721121));
#15553=CARTESIAN_POINT('Ctrl Pts',(0.259205604618467,-7.40800140771156,
26.9227686130061));
#15554=CARTESIAN_POINT('Ctrl Pts',(0.229333295950648,-7.39994545613123,
26.9230381673609));
#15555=CARTESIAN_POINT('Ctrl Pts',(0.156558955122424,-7.36980200110025,
26.923581519186));
#15556=CARTESIAN_POINT('Ctrl Pts',(0.115977709440296,-7.34202846079804,
26.9237692730492));
#15557=CARTESIAN_POINT('Ctrl Pts',(0.0518946969700347,-7.27794557643884,
26.9239690532275));
#15558=CARTESIAN_POINT('Ctrl Pts',(0.0241213194106565,-7.23736545441392,
26.9239954921155));
#15559=CARTESIAN_POINT('Ctrl Pts',(-0.0127078805578039,-7.14845207902969,
26.9240032983076));
#15560=CARTESIAN_POINT('Ctrl Pts',(-0.0217637041830137,-7.10011882686834,
26.9239912037792));
#15561=CARTESIAN_POINT('Ctrl Pts',(-0.0217637041830158,-7.01443642784654,
26.9239912037792));
#15562=CARTESIAN_POINT('Ctrl Pts',(-0.0146546819566494,-6.97164118553968,
26.924));
#15563=CARTESIAN_POINT('Ctrl Pts',(-3.3784413704887E-13,-6.93137777777542,
26.924));
#15564=CARTESIAN_POINT('',(0.274225953490026,-6.17794816273243,26.9226034425802));
#15565=CARTESIAN_POINT('Origin',(2.33843412203449E-6,-6.93137130119064,
-203.230148290915));
#15566=CARTESIAN_POINT('',(0.613341870778106,-5.94049664112042,26.917012979704));
#15567=CARTESIAN_POINT('Ctrl Pts',(0.613341870778106,-5.94049664112043,
26.9170129797039));
#15568=CARTESIAN_POINT('Ctrl Pts',(0.568034460510535,-5.94049664112043,
26.9180453725551));
#15569=CARTESIAN_POINT('Ctrl Pts',(0.519703302410495,-5.94955040320058,
26.9190204417453));
#15570=CARTESIAN_POINT('Ctrl Pts',(0.430788744733556,-5.98637789273599,
26.9205901518345));
#15571=CARTESIAN_POINT('Ctrl Pts',(0.390205518515635,-6.01415175978563,
26.9211913305823));
#15572=CARTESIAN_POINT('Ctrl Pts',(0.326121343092076,-6.07823593520919,
26.922043897507));
#15573=CARTESIAN_POINT('Ctrl Pts',(0.298347895423894,-6.11881559083292,
26.9223532343272));
#15574=CARTESIAN_POINT('Ctrl Pts',(0.277923984350046,-6.16812272243846,
26.9225655964655));
#15575=CARTESIAN_POINT('Ctrl Pts',(0.276020647354955,-6.17301728186366,
26.9225851623408));
#15576=CARTESIAN_POINT('Ctrl Pts',(0.274225953490012,-6.17794816273242,
26.9226034425802));
#15577=CARTESIAN_POINT('',(2.34365910677381,-5.9404966411204,26.8218015426115));
#15578=CARTESIAN_POINT('Origin',(0.,-5.94049664112042,0.));
#15579=CARTESIAN_POINT('',(2.68277502406178,-6.42480436244983,26.7900073566664));
#15580=CARTESIAN_POINT('Ctrl Pts',(2.6827750240618,-6.42480436244982,26.790007356667));
#15581=CARTESIAN_POINT('Ctrl Pts',(2.69742378804539,-6.384557214182,26.7885404164894));
#15582=CARTESIAN_POINT('Ctrl Pts',(2.70453872824448,-6.34175941776375,26.7878189904932));
#15583=CARTESIAN_POINT('Ctrl Pts',(2.70453872824448,-6.30137626259108,26.7878189904932));
#15584=CARTESIAN_POINT('Ctrl Pts',(2.70453872824448,-6.25601754641993,26.7878189904932));
#15585=CARTESIAN_POINT('Ctrl Pts',(2.695463613825,-6.20765596068026,26.7887400748593));
#15586=CARTESIAN_POINT('Ctrl Pts',(2.65861246360117,-6.11874469509012,26.7924224111967));
#15587=CARTESIAN_POINT('Ctrl Pts',(2.63083784468254,-6.07819414543192,26.7951768375626));
#15588=CARTESIAN_POINT('Ctrl Pts',(2.56676708896078,-6.01412338971015,26.8013902816038));
#15589=CARTESIAN_POINT('Ctrl Pts',(2.52617139162328,-5.98635509740792,26.8052649156946));
#15590=CARTESIAN_POINT('Ctrl Pts',(2.43726320056164,-5.94954200849695,26.8134950573699));
#15591=CARTESIAN_POINT('Ctrl Pts',(2.38895033976021,-5.94049664112042,26.8178440451825));
#15592=CARTESIAN_POINT('Ctrl Pts',(2.34365910677381,-5.94049664112042,26.8218015426115));
#15593=CARTESIAN_POINT('',(2.51551931327143,-6.88433565112087,26.8062294734736));
#15594=CARTESIAN_POINT('Origin',(0.000112111321052266,-13.7953601167503,
0.00114962729787838));
#15595=CARTESIAN_POINT('',(1.51616036150637,-6.88433565112087,26.8812766392927));
#15596=CARTESIAN_POINT('Origin',(0.,-6.88433565112087,0.));
#15597=CARTESIAN_POINT('',(1.57625656123139,-6.71922269938127,26.8778196893491));
#15598=CARTESIAN_POINT('Origin',(-0.0199859957526316,-11.1048629590776,
-0.347501760955415));
#15599=CARTESIAN_POINT('',(1.41974152248314,-6.49569605876778,26.8865414289257));
#15600=CARTESIAN_POINT('Ctrl Pts',(1.57625656123142,-6.71922269938128,26.8778196893491));
#15601=CARTESIAN_POINT('Ctrl Pts',(1.57924172308355,-6.71102103459914,26.8776446237742));
#15602=CARTESIAN_POINT('Ctrl Pts',(1.58159845093676,-6.70252742481101,26.8775068990936));
#15603=CARTESIAN_POINT('Ctrl Pts',(1.58326847821739,-6.69389620881209,26.877408610663));
#15604=CARTESIAN_POINT('Ctrl Pts',(1.58493854579429,-6.68526478454967,26.8773103198609));
#15605=CARTESIAN_POINT('Ctrl Pts',(1.58592165516389,-6.67649682270982,26.877251467212));
#15606=CARTESIAN_POINT('Ctrl Pts',(1.58621047322079,-6.66775714231041,26.877234148224));
#15607=CARTESIAN_POINT('Ctrl Pts',(1.58624861877,-6.66660285191615,26.8772318608244));
#15608=CARTESIAN_POINT('Ctrl Pts',(1.58627472784398,-6.66544905600654,26.8772302979262));
#15609=CARTESIAN_POINT('Ctrl Pts',(1.58628885146083,-6.66429613218638,26.8772294643573));
#15610=CARTESIAN_POINT('Ctrl Pts',(1.58639578526895,-6.65556702717844,26.8772231531769));
#15611=CARTESIAN_POINT('Ctrl Pts',(1.58581283069008,-6.64677083102588,26.8772585712934));
#15612=CARTESIAN_POINT('Ctrl Pts',(1.5845363581515,-6.638072469517,26.8773339031591));
#15613=CARTESIAN_POINT('Ctrl Pts',(1.58325979836866,-6.62937351349312,26.8774092401736));
#15614=CARTESIAN_POINT('Ctrl Pts',(1.5812897718651,-6.62077349426359,26.8775244963936));
#15615=CARTESIAN_POINT('Ctrl Pts',(1.57867417248658,-6.61243030664534,26.8776778558992));
#15616=CARTESIAN_POINT('Ctrl Pts',(1.57832878928513,-6.61132861008064,26.8776981066293));
#15617=CARTESIAN_POINT('Ctrl Pts',(1.57797222019385,-6.61023136807441,26.8777190217483));
#15618=CARTESIAN_POINT('Ctrl Pts',(1.57760463878763,-6.6091389196094,26.8777405970752));
#15619=CARTESIAN_POINT('Ctrl Pts',(1.57481834327256,-6.60085807567399,26.8779041397233));
#15620=CARTESIAN_POINT('Ctrl Pts',(1.57135790941734,-6.59274300000671,26.8781076660283));
#15621=CARTESIAN_POINT('Ctrl Pts',(1.56727477083692,-6.58495054121813,26.8783458075278));
#15622=CARTESIAN_POINT('Ctrl Pts',(1.56319121958177,-6.57715729486115,26.8785839730957));
#15623=CARTESIAN_POINT('Ctrl Pts',(1.55848533749749,-6.56968770889263,26.8788567608554));
#15624=CARTESIAN_POINT('Ctrl Pts',(1.55325482389809,-6.56267489316859,26.8791588007165));
#15625=CARTESIAN_POINT('Ctrl Pts',(1.55257588632846,-6.56176460702299,26.8791980064667));
#15626=CARTESIAN_POINT('Ctrl Pts',(1.55188816612293,-6.56086197263135,26.8792377050819));
#15627=CARTESIAN_POINT('Ctrl Pts',(1.55119192582283,-6.55996723921877,26.8792778848177));
#15628=CARTESIAN_POINT('Ctrl Pts',(1.54581973584129,-6.55306347643089,26.8795879116488));
#15629=CARTESIAN_POINT('Ctrl Pts',(1.53986492057117,-6.54654020750865,26.8799304894413));
#15630=CARTESIAN_POINT('Ctrl Pts',(1.53342806699248,-6.54052854531033,26.8802977131248));
#15631=CARTESIAN_POINT('Ctrl Pts',(1.52699052246563,-6.53451623780498,26.8806649762271));
#15632=CARTESIAN_POINT('Ctrl Pts',(1.52007163158253,-6.52901640454359,26.881056890512));
#15633=CARTESIAN_POINT('Ctrl Pts',(1.51280778436154,-6.52412244747976,26.8814655483633));
#15634=CARTESIAN_POINT('Ctrl Pts',(1.51187416217166,-6.52349342724129,26.8815180731517));
#15635=CARTESIAN_POINT('Ctrl Pts',(1.51093487951499,-6.52287435659452,26.8815708745431));
#15636=CARTESIAN_POINT('Ctrl Pts',(1.5099902572712,-6.52226537984406,26.8816239357471));
#15637=CARTESIAN_POINT('Ctrl Pts',(1.50215617445506,-6.51721492255531,26.88206399088));
#15638=CARTESIAN_POINT('Ctrl Pts',(1.4938402503677,-6.51279092222325,26.8825278684243));
#15639=CARTESIAN_POINT('Ctrl Pts',(1.48520349091112,-6.50909940822249,26.8830050067835));
#15640=CARTESIAN_POINT('Ctrl Pts',(1.47656673145454,-6.50540789422174,26.8834821451427));
#15641=CARTESIAN_POINT('Ctrl Pts',(1.46761038526522,-6.50244943200829,26.8839725443169));
#15642=CARTESIAN_POINT('Ctrl Pts',(1.45852086118223,-6.50027335941163,26.8844656427098));
#15643=CARTESIAN_POINT('Ctrl Pts',(1.45040284645242,-6.4983298704862,26.8849060376062));
#15644=CARTESIAN_POINT('Ctrl Pts',(1.44207893045424,-6.4969868112561,26.8853538739836));
#15645=CARTESIAN_POINT('Ctrl Pts',(1.43370310795781,-6.49628224298282,26.8858005302961));
#15646=CARTESIAN_POINT('Ctrl Pts',(1.42905591253747,-6.49589132418598,26.886048350635));
#15647=CARTESIAN_POINT('Ctrl Pts',(1.42439300666299,-6.49569605876777,26.8862958077011));
#15648=CARTESIAN_POINT('Ctrl Pts',(1.41974152248314,-6.49569605876777,26.8865414289257));
#15649=CARTESIAN_POINT('',(1.27456057433151,-6.49569605876777,26.8938147413557));
#15650=CARTESIAN_POINT('Origin',(0.,-6.49569605876778,0.));
#15651=CARTESIAN_POINT('',(1.11804553558315,-6.60528906874258,26.900776014464));
#15652=CARTESIAN_POINT('Ctrl Pts',(1.27456057433151,-6.49569605876777,26.8938147413557));
#15653=CARTESIAN_POINT('Ctrl Pts',(1.26581104241068,-6.49569605876777,26.8942294020699));
#15654=CARTESIAN_POINT('Ctrl Pts',(1.25700253962824,-6.49638982924727,26.8946422411103));
#15655=CARTESIAN_POINT('Ctrl Pts',(1.24830041528794,-6.49777920045897,26.8950461000855));
#15656=CARTESIAN_POINT('Ctrl Pts',(1.23959807403636,-6.49916860630247,26.8954499691274));
#15657=CARTESIAN_POINT('Ctrl Pts',(1.23100320364805,-6.50125349026164,26.8958448576564));
#15658=CARTESIAN_POINT('Ctrl Pts',(1.22267356065485,-6.50398424031694,26.8962236067463));
#15659=CARTESIAN_POINT('Ctrl Pts',(1.22157435894952,-6.50434459731184,26.8962735874772));
#15660=CARTESIAN_POINT('Ctrl Pts',(1.22047975154766,-6.50471613119169,26.8963232871537));
#15661=CARTESIAN_POINT('Ctrl Pts',(1.21939007580004,-6.50509866503012,26.8963726893245));
#15662=CARTESIAN_POINT('Ctrl Pts',(1.21113910606108,-6.5079951919391,26.8967467600669));
#15663=CARTESIAN_POINT('Ctrl Pts',(1.20306165874366,-6.51156526108334,26.8971086735187));
#15664=CARTESIAN_POINT('Ctrl Pts',(1.19531434190978,-6.51575602041357,26.8974529141699));
#15665=CARTESIAN_POINT('Ctrl Pts',(1.18756694845903,-6.5199468211882,26.8977971582255));
#15666=CARTESIAN_POINT('Ctrl Pts',(1.1801506662191,-6.52475781698821,26.8981237291309));
#15667=CARTESIAN_POINT('Ctrl Pts',(1.17319793803882,-6.53009011176886,26.8984271112124));
#15668=CARTESIAN_POINT('Ctrl Pts',(1.17226845360873,-6.53080296647089,26.8984676692371));
#15669=CARTESIAN_POINT('Ctrl Pts',(1.17134720637668,-6.53152507802084,26.8985078128305));
#15670=CARTESIAN_POINT('Ctrl Pts',(1.17043446638727,-6.53225615696063,26.8985475288145));
#15671=CARTESIAN_POINT('Ctrl Pts',(1.16315500731248,-6.53808679798041,26.8988642793493));
#15672=CARTESIAN_POINT('Ctrl Pts',(1.15631558875019,-6.54457532770192,26.8991583144776));
#15673=CARTESIAN_POINT('Ctrl Pts',(1.15006885402281,-6.55160333336104,26.8994253521022));
#15674=CARTESIAN_POINT('Ctrl Pts',(1.14382211929544,-6.55863133902016,26.8996923897268));
#15675=CARTESIAN_POINT('Ctrl Pts',(1.13816901044215,-6.56619782081524,26.8999324298477));
#15676=CARTESIAN_POINT('Ctrl Pts',(1.13321664410958,-6.57414193061837,26.9001411903677));
#15677=CARTESIAN_POINT('Ctrl Pts',(1.12892028114709,-6.58103374290287,26.9003222979245));
#15678=CARTESIAN_POINT('Ctrl Pts',(1.12509800042944,-6.58829608747506,26.9004820858555));
#15679=CARTESIAN_POINT('Ctrl Pts',(1.12183355869422,-6.59579812231385,26.9006182594057));
#15680=CARTESIAN_POINT('Ctrl Pts',(1.12047334394055,-6.59892404070906,26.9006749996655));
#15681=CARTESIAN_POINT('Ctrl Pts',(1.11920945065392,-6.60209123836739,26.9007276400213));
#15682=CARTESIAN_POINT('Ctrl Pts',(1.11804553558312,-6.60528906874257,26.900776014464));
#15683=CARTESIAN_POINT('',(1.03031472940818,-6.84632747769874,26.9042789823173));
#15684=CARTESIAN_POINT('Origin',(-0.000189062495069697,-9.67761327915856,
-0.00486750830971161));
#15685=CARTESIAN_POINT('',(1.16364912077505,-7.06823316954214,26.8988419216091));
#15686=CARTESIAN_POINT('Ctrl Pts',(1.0303147294082,-6.84632747769875,26.9042789823174));
#15687=CARTESIAN_POINT('Ctrl Pts',(1.02355144389689,-6.86490945192241,26.9045379861987));
#15688=CARTESIAN_POINT('Ctrl Pts',(1.02026994286236,-6.88466135938939,26.9046617753075));
#15689=CARTESIAN_POINT('Ctrl Pts',(1.02026994286236,-6.92421126357124,26.9046617753075));
#15690=CARTESIAN_POINT('Ctrl Pts',(1.02445101377191,-6.9465211005437,26.9045044455911));
#15691=CARTESIAN_POINT('Ctrl Pts',(1.04145074477865,-6.987558080578,26.9038513690675));
#15692=CARTESIAN_POINT('Ctrl Pts',(1.05426948991939,-7.00628517865852,26.9033550096459));
#15693=CARTESIAN_POINT('Ctrl Pts',(1.08384689122566,-7.03586257996479,26.9021796716557));
#15694=CARTESIAN_POINT('Ctrl Pts',(1.10257970657431,-7.04868104393975,26.9014223859628));
#15695=CARTESIAN_POINT('Ctrl Pts',(1.13616675375296,-7.06259126795534,26.90001980511));
#15696=CARTESIAN_POINT('Ctrl Pts',(1.14995147001454,-7.06630809027082,26.8994344846389));
#15697=CARTESIAN_POINT('Ctrl Pts',(1.16364912077505,-7.06823316954215,26.8988419216092));
#15698=CARTESIAN_POINT('',(1.94474447683868,-7.17800896286548,26.8536728385484));
#15699=CARTESIAN_POINT('Origin',(9.87539452229624E-5,-6.90470682992473,
-0.529111024329425));
#15700=CARTESIAN_POINT('',(2.23363565813339,-7.65880462852638,26.8311879674888));
#15701=CARTESIAN_POINT('Ctrl Pts',(2.23363565813343,-7.6588046285264,26.8311879674888));
#15702=CARTESIAN_POINT('Ctrl Pts',(2.24828626275416,-7.61855242314961,26.82996833782));
#15703=CARTESIAN_POINT('Ctrl Pts',(2.25539936231613,-7.57575548944259,26.8293672999656));
#15704=CARTESIAN_POINT('Ctrl Pts',(2.25539936231613,-7.53537652866759,26.8293672999656));
#15705=CARTESIAN_POINT('Ctrl Pts',(2.25539936231613,-7.4900321919393,26.8293672999656));
#15706=CARTESIAN_POINT('Ctrl Pts',(2.24633033032357,-7.44167964383524,26.8301345087731));
#15707=CARTESIAN_POINT('Ctrl Pts',(2.20948623080687,-7.35276791028762,26.8331937776234));
#15708=CARTESIAN_POINT('Ctrl Pts',(2.18171215147441,-7.31220808422858,26.8354791168319));
#15709=CARTESIAN_POINT('Ctrl Pts',(2.11763929243676,-7.24813522519093,26.8406112881533));
#15710=CARTESIAN_POINT('Ctrl Pts',(2.07705023376966,-7.22036567768755,26.8438005107346));
#15711=CARTESIAN_POINT('Ctrl Pts',(2.00428320831623,-7.19023141536068,26.8493096934061));
#15712=CARTESIAN_POINT('Ctrl Pts',(1.97442026744516,-7.18217962324777,26.8515237161465));
#15713=CARTESIAN_POINT('Ctrl Pts',(1.9447444768387,-7.17800896286548,26.8536728385486));
#15714=CARTESIAN_POINT('',(1.93509359427102,-8.47904220774527,26.8543700127446));
#15715=CARTESIAN_POINT('Origin',(0.011017235378798,-13.7653985140978,-201.413368973554));
#15716=CARTESIAN_POINT('',(1.59597767698316,-8.71649372935708,26.8766558793046));
#15717=CARTESIAN_POINT('Ctrl Pts',(1.59597767698316,-8.71649372935709,26.8766558793048));
#15718=CARTESIAN_POINT('Ctrl Pts',(1.64130934118138,-8.71649372935708,26.8739640144967));
#15719=CARTESIAN_POINT('Ctrl Pts',(1.6896593272796,-8.70743151832439,26.8709659961303));
#15720=CARTESIAN_POINT('Ctrl Pts',(1.77860802648519,-8.67057108473292,26.8652250259622));
#15721=CARTESIAN_POINT('Ctrl Pts',(1.81920709137776,-8.64277269368148,26.8624886082932));
#15722=CARTESIAN_POINT('Ctrl Pts',(1.88325421352363,-8.57867124997308,26.8580743475323));
#15723=CARTESIAN_POINT('Ctrl Pts',(1.91099991290959,-8.53811969476632,26.8561016470336));
#15724=CARTESIAN_POINT('Ctrl Pts',(1.93140462620437,-8.4888443320221,26.8546356557978));
#15725=CARTESIAN_POINT('Ctrl Pts',(1.93330314905799,-8.48396141553878,26.8544990300728));
#15726=CARTESIAN_POINT('Ctrl Pts',(1.93509359427101,-8.47904220774526,26.8543700127449));
#15727=CARTESIAN_POINT('',(-0.134339559012431,-8.71649372935709,26.9236648486584));
#15728=CARTESIAN_POINT('Origin',(0.,-8.71649372935708,0.));
#15729=CARTESIAN_POINT('',(-0.473455476300511,-8.23218600802749,26.9198368477961));
#15730=CARTESIAN_POINT('Ctrl Pts',(-0.134339559012431,-8.7164937293571,
26.9236648486584));
#15731=CARTESIAN_POINT('Ctrl Pts',(-0.17965419798474,-8.7164937293571,26.9234387446473));
#15732=CARTESIAN_POINT('Ctrl Pts',(-0.227988226664942,-8.7074372901076,
26.9230714068759));
#15733=CARTESIAN_POINT('Ctrl Pts',(-0.316901866605793,-8.67060716866254,
26.9221716400847));
#15734=CARTESIAN_POINT('Ctrl Pts',(-0.357481564104588,-8.64283353526289,
26.921645747504));
#15735=CARTESIAN_POINT('Ctrl Pts',(-0.421561817763482,-8.57875212678267,
26.9207185710247));
#15736=CARTESIAN_POINT('Ctrl Pts',(-0.449334417014175,-8.53817306977746,
26.9202565695887));
#15737=CARTESIAN_POINT('Ctrl Pts',(-0.486163125349526,-8.44926085508519,
26.9196166504351));
#15738=CARTESIAN_POINT('Ctrl Pts',(-0.495219180483252,-8.40092762807852,
26.9194452759206));
#15739=CARTESIAN_POINT('Ctrl Pts',(-0.495219180483254,-8.31524416266397,
26.9194452759206));
#15740=CARTESIAN_POINT('Ctrl Pts',(-0.488109987951914,-8.27244894788268,
26.9195791100233));
#15741=CARTESIAN_POINT('Ctrl Pts',(-0.473455476300561,-8.23218600802747,
26.9198368477961));
#15742=CARTESIAN_POINT('',(-0.306199765510384,-7.77265471935663,26.9222587778886));
#15743=CARTESIAN_POINT('Origin',(8.71111081393594E-7,-6.93137537062405,
-0.000135688494280473));
#15744=CARTESIAN_POINT('',(0.693159186254899,-7.77265471935663,26.9150758189998));
#15745=CARTESIAN_POINT('Origin',(0.,-7.77265471935663,0.));
#15746=CARTESIAN_POINT('',(0.633062986529875,-7.9377676710961,26.9165563780935));
#15747=CARTESIAN_POINT('Origin',(0.00521753124544971,-9.66275886061376,
0.2131092784871));
#15748=CARTESIAN_POINT('',(0.789578025278126,-8.16129431170977,26.9124198566758));
#15749=CARTESIAN_POINT('Ctrl Pts',(0.633062986529795,-7.93776767109607,
26.9165563780935));
#15750=CARTESIAN_POINT('Ctrl Pts',(0.626299444360304,-7.95635035048225,
26.916715452982));
#15751=CARTESIAN_POINT('Ctrl Pts',(0.623018199983921,-7.97610210840517,
26.9167907508025));
#15752=CARTESIAN_POINT('Ctrl Pts',(0.623018199983921,-8.01564754896317,
26.9167907508025));
#15753=CARTESIAN_POINT('Ctrl Pts',(0.627197630926004,-8.0379541898489,26.916695234733));
#15754=CARTESIAN_POINT('Ctrl Pts',(0.644193571406133,-8.07898830888383,
26.9162934428526));
#15755=CARTESIAN_POINT('Ctrl Pts',(0.657010113747562,-8.09771576748714,
26.915986558688));
#15756=CARTESIAN_POINT('Ctrl Pts',(0.68658516522624,-8.12729476128226,26.9152483865216));
#15757=CARTESIAN_POINT('Ctrl Pts',(0.705317145235529,-8.14011531833232,
26.9147679862365));
#15758=CARTESIAN_POINT('Ctrl Pts',(0.746357230199947,-8.15711512726127,
26.9136608016588));
#15759=CARTESIAN_POINT('Ctrl Pts',(0.768665346685277,-8.16129431170977,
26.9130334095096));
#15760=CARTESIAN_POINT('Ctrl Pts',(0.789578025278126,-8.16129431170977,
26.9124198566758));
#15761=CARTESIAN_POINT('',(0.934758973429761,-8.16129431170976,26.907768425895));
#15762=CARTESIAN_POINT('Origin',(0.,-8.16129431170977,0.));
#15763=CARTESIAN_POINT('',(1.09127401217801,-8.05170130173499,26.9018753441158));
#15764=CARTESIAN_POINT('Ctrl Pts',(0.934758973429761,-8.16129431170975,
26.907768425895));
#15765=CARTESIAN_POINT('Ctrl Pts',(0.943507416250645,-8.16129431170975,
26.9074645104866));
#15766=CARTESIAN_POINT('Ctrl Pts',(0.952314450605376,-8.16060071259162,
26.9071541284652));
#15767=CARTESIAN_POINT('Ctrl Pts',(0.961014765045493,-8.15921186725762,
26.9068433912338));
#15768=CARTESIAN_POINT('Ctrl Pts',(0.969715507217545,-8.15782295364408,
26.9065326387256));
#15769=CARTESIAN_POINT('Ctrl Pts',(0.978308432019303,-8.1557388841085,26.9062215309723));
#15770=CARTESIAN_POINT('Ctrl Pts',(0.986635868110279,-8.15300944716532,
26.9059161802782));
#15771=CARTESIAN_POINT('Ctrl Pts',(0.987735619734303,-8.15264898775403,
26.9058758545503));
#15772=CARTESIAN_POINT('Ctrl Pts',(0.988830765541148,-8.15227734300836,
26.9058356292302));
#15773=CARTESIAN_POINT('Ctrl Pts',(0.989920967675642,-8.15189469064312,
26.9057955183963));
#15774=CARTESIAN_POINT('Ctrl Pts',(0.998174225169999,-8.14899786224657,
26.9054918636611));
#15775=CARTESIAN_POINT('Ctrl Pts',(1.00625345218897,-8.14542729599591,26.9051909040077));
#15776=CARTESIAN_POINT('Ctrl Pts',(1.01400208488805,-8.14123603824502,26.9048988998938));
#15777=CARTESIAN_POINT('Ctrl Pts',(1.02175096540805,-8.13704464644708,26.9046068864408));
#15778=CARTESIAN_POINT('Ctrl Pts',(1.02916825690228,-8.13223303216125,26.9043238291002));
#15779=CARTESIAN_POINT('Ctrl Pts',(1.03612160509544,-8.12690026225726,26.9040559889302));
#15780=CARTESIAN_POINT('Ctrl Pts',(1.03704279892234,-8.1261937659652,26.9040205049152));
#15781=CARTESIAN_POINT('Ctrl Pts',(1.03795589653766,-8.12547818132169,26.9039852879844));
#15782=CARTESIAN_POINT('Ctrl Pts',(1.03886063534056,-8.12475379032632,26.9039503526961));
#15783=CARTESIAN_POINT('Ctrl Pts',(1.04614074014404,-8.11892487887908,26.9036692411104));
#15784=CARTESIAN_POINT('Ctrl Pts',(1.05298067479204,-8.11243833566999,26.9034025976216));
#15785=CARTESIAN_POINT('Ctrl Pts',(1.0592280303383,-8.1054125297409,26.9031566705941));
#15786=CARTESIAN_POINT('Ctrl Pts',(1.06547538588456,-8.09838672381181,26.9029107435666));
#15787=CARTESIAN_POINT('Ctrl Pts',(1.07112922323023,-8.09082265301925,26.9026855330005));
#15788=CARTESIAN_POINT('Ctrl Pts',(1.07608258887272,-8.08288101850931,26.9024872872602));
#15789=CARTESIAN_POINT('Ctrl Pts',(1.08038264103286,-8.07598682876151,26.9023151887144));
#15790=CARTESIAN_POINT('Ctrl Pts',(1.0842081381144,-8.06872179489345,26.9021613447548));
#15791=CARTESIAN_POINT('Ctrl Pts',(1.08747530132548,-8.06121680433596,26.9020292293634));
#15792=CARTESIAN_POINT('Ctrl Pts',(1.08883958988695,-8.05808290127999,26.9019740611622));
#15793=CARTESIAN_POINT('Ctrl Pts',(1.09010705367343,-8.0549074938759,26.9019226817632));
#15794=CARTESIAN_POINT('Ctrl Pts',(1.09127401217806,-8.05170130173501,26.9018753441158));
#15795=CARTESIAN_POINT('',(1.20332092872488,-7.74385492860298,26.8970963998438));
#15796=CARTESIAN_POINT('Origin',(-0.000120088806767477,-11.0502819126076,
-0.00289697876735051));
#15797=CARTESIAN_POINT('',(1.06998653735801,-7.52194923675958,26.9027304341004));
#15798=CARTESIAN_POINT('Ctrl Pts',(1.20332092872487,-7.74385492860298,26.8970963998438));
#15799=CARTESIAN_POINT('Ctrl Pts',(1.20630820149836,-7.73564746411204,26.8969627553866));
#15800=CARTESIAN_POINT('Ctrl Pts',(1.20866602936409,-7.72714799377406,26.8968575489923));
#15801=CARTESIAN_POINT('Ctrl Pts',(1.21033621989448,-7.71851099422374,26.8967824609427));
#15802=CARTESIAN_POINT('Ctrl Pts',(1.21200646802853,-7.70987369678953,26.8967073703033));
#15803=CARTESIAN_POINT('Ctrl Pts',(1.21298880759412,-7.70109993608949,26.8966624000862));
#15804=CARTESIAN_POINT('Ctrl Pts',(1.21327598473685,-7.69235464349173,26.8966492307471));
#15805=CARTESIAN_POINT('Ctrl Pts',(1.21331392930616,-7.69119913244401,26.896647490689));
#15806=CARTESIAN_POINT('Ctrl Pts',(1.21333981219762,-7.69004411950586,26.8966463058171));
#15807=CARTESIAN_POINT('Ctrl Pts',(1.21335368467758,-7.68888998297058,26.8966456800077));
#15808=CARTESIAN_POINT('Ctrl Pts',(1.21345867250687,-7.68015540271682,26.8966409438417));
#15809=CARTESIAN_POINT('Ctrl Pts',(1.21287289959885,-7.67135384905538,26.8966681695819));
#15810=CARTESIAN_POINT('Ctrl Pts',(1.21159274133503,-7.66265035304505,26.8967258968327));
#15811=CARTESIAN_POINT('Ctrl Pts',(1.21031250598962,-7.65394633297508,26.8967836275594));
#15812=CARTESIAN_POINT('Ctrl Pts',(1.20833794759953,-7.64534147114135,26.89687186347));
#15813=CARTESIAN_POINT('Ctrl Pts',(1.20571696461041,-7.63699376730395,26.8969891439052));
#15814=CARTESIAN_POINT('Ctrl Pts',(1.20537069753749,-7.63589092345288,26.8970046382267));
#15815=CARTESIAN_POINT('Ctrl Pts',(1.20501321852504,-7.63479254431635,26.8970206394901));
#15816=CARTESIAN_POINT('Ctrl Pts',(1.20464470142482,-7.63369896962983,26.8970371443274));
#15817=CARTESIAN_POINT('Ctrl Pts',(1.20185378621253,-7.62541692728621,26.897162141516));
#15818=CARTESIAN_POINT('Ctrl Pts',(1.19838830743005,-7.61730076007746,26.8973175753973));
#15819=CARTESIAN_POINT('Ctrl Pts',(1.19429962640976,-7.60950741081202,26.8974991615228));
#15820=CARTESIAN_POINT('Ctrl Pts',(1.19021062312795,-7.60171344729063,26.8976807619605));
#15821=CARTESIAN_POINT('Ctrl Pts',(1.18549881836612,-7.59424333125702,26.897888518765));
#15822=CARTESIAN_POINT('Ctrl Pts',(1.18026184976452,-7.58723028770478,26.8981181464746));
#15823=CARTESIAN_POINT('Ctrl Pts',(1.17957707223917,-7.58631327349785,26.8981481722216));
#15824=CARTESIAN_POINT('Ctrl Pts',(1.1788833732658,-7.58540402928745,26.8981785719121));
#15825=CARTESIAN_POINT('Ctrl Pts',(1.17818102115397,-7.58450281008953,26.8982093359649));
#15826=CARTESIAN_POINT('Ctrl Pts',(1.17280483184219,-7.5776043827368,26.8984448209439));
#15827=CARTESIAN_POINT('Ctrl Pts',(1.16684619617214,-7.57108629836871,26.8987046007507));
#15828=CARTESIAN_POINT('Ctrl Pts',(1.16040560201427,-7.56507973579265,26.8989824596729));
#15829=CARTESIAN_POINT('Ctrl Pts',(1.15396448410204,-7.55907268475805,26.8992603411909));
#15830=CARTESIAN_POINT('Ctrl Pts',(1.14704212408627,-7.55357799705623,26.8995563047649));
#15831=CARTESIAN_POINT('Ctrl Pts',(1.13977483038196,-7.54868915698535,26.899864133166));
#15832=CARTESIAN_POINT('Ctrl Pts',(1.13882983230903,-7.54805343966968,26.8999041614431));
#15833=CARTESIAN_POINT('Ctrl Pts',(1.13787904090127,-7.54742790579136,26.8999443903418));
#15834=CARTESIAN_POINT('Ctrl Pts',(1.13692278833406,-7.54681270490492,26.8999848061921));
#15835=CARTESIAN_POINT('Ctrl Pts',(1.12908371336223,-7.54176947047405,26.9003161233476));
#15836=CARTESIAN_POINT('Ctrl Pts',(1.12076286306026,-7.53735290381581,26.9006644645301));
#15837=CARTESIAN_POINT('Ctrl Pts',(1.11212178203379,-7.53366928400077,26.9010216830877));
#15838=CARTESIAN_POINT('Ctrl Pts',(1.10348070100732,-7.52998566418573,26.9013789016454));
#15839=CARTESIAN_POINT('Ctrl Pts',(1.09452064817113,-7.52703555982621,26.9017449975782));
#15840=CARTESIAN_POINT('Ctrl Pts',(1.08542866866471,-7.52486818744594,26.9021118242343));
#15841=CARTESIAN_POINT('Ctrl Pts',(1.08036776450329,-7.52366175446939,26.9023160123926));
#15842=CARTESIAN_POINT('Ctrl Pts',(1.07519179640413,-7.52268078821074,26.9025234083817));
#15843=CARTESIAN_POINT('Ctrl Pts',(1.06998653735802,-7.52194923675956,26.9027304341004));
#15844=CARTESIAN_POINT('Origin',(7.69056924636302E-6,-7.37157351664769,
-0.531259473272554));
#15845=CARTESIAN_POINT('Origin',(2.80821735451831,-8.35561410788639,27.4319999999998));
#15846=CARTESIAN_POINT('',(2.80821735451788,-8.71649372935709,25.9256866653046));
#15847=CARTESIAN_POINT('',(2.80821735451831,-8.71649372935708,27.4319999999998));
#15848=CARTESIAN_POINT('',(2.4691014372298,-8.23218600802769,25.9601781941197));
#15849=CARTESIAN_POINT('Ctrl Pts',(2.80821735451831,-8.71649372935709,25.9256866653048));
#15850=CARTESIAN_POINT('Ctrl Pts',(2.76291647430916,-8.71649372935709,25.9305935639965));
#15851=CARTESIAN_POINT('Ctrl Pts',(2.71456192154659,-8.70744327429823,25.9356987402673));
#15852=CARTESIAN_POINT('Ctrl Pts',(2.62554938695351,-8.67055460416721,25.9448608781866));
#15853=CARTESIAN_POINT('Ctrl Pts',(2.58489292205166,-8.6427143866552,25.9489245135623));
#15854=CARTESIAN_POINT('Ctrl Pts',(2.52086167203555,-8.5785552949802,25.9552229620713));
#15855=CARTESIAN_POINT('Ctrl Pts',(2.49315120182095,-8.5380356743044,25.9578861197208));
#15856=CARTESIAN_POINT('Ctrl Pts',(2.45638866397115,-8.44921368708084,25.9613907456984));
#15857=CARTESIAN_POINT('Ctrl Pts',(2.44733773304761,-8.40091111635172,25.9622389596541));
#15858=CARTESIAN_POINT('Ctrl Pts',(2.44733773304761,-8.31522953260126,25.9622389596541));
#15859=CARTESIAN_POINT('Ctrl Pts',(2.45445256771952,-8.27243344622907,25.9615714644005));
#15860=CARTESIAN_POINT('Ctrl Pts',(2.46910143723022,-8.23218600802784,25.9601781941197));
#15861=CARTESIAN_POINT('',(2.46910143723034,-8.23218600802769,27.432));
#15862=CARTESIAN_POINT('Origin',(3.73213493880821,-7.994734486418,53.8479999999997));
#15863=CARTESIAN_POINT('',(3.57561990006094,-7.93776767109861,26.6855151408078));
#15864=CARTESIAN_POINT('',(3.7321349388092,-8.16129431171214,26.6640759224563));
#15865=CARTESIAN_POINT('Ctrl Pts',(3.73213493880821,-8.16129431171213,26.6640759224566));
#15866=CARTESIAN_POINT('Ctrl Pts',(3.71121764562174,-8.16129431171213,26.6670036879247));
#15867=CARTESIAN_POINT('Ctrl Pts',(3.68888741410261,-8.15711485847784,26.6701013442994));
#15868=CARTESIAN_POINT('Ctrl Pts',(3.64777149434979,-8.1400619989865,26.6757564173205));
#15869=CARTESIAN_POINT('Ctrl Pts',(3.62898539697396,-8.12718980443669,26.6783145130552));
#15870=CARTESIAN_POINT('Ctrl Pts',(3.59945898034547,-8.09755577679515,26.6823141930242));
#15871=CARTESIAN_POINT('Ctrl Pts',(3.58669338059613,-8.07887895891479,26.684030229594));
#15872=CARTESIAN_POINT('Ctrl Pts',(3.5697519397839,-8.03791928644474,26.6863023153227));
#15873=CARTESIAN_POINT('Ctrl Pts',(3.56557511351408,-8.01563688170508,26.6868591278533));
#15874=CARTESIAN_POINT('Ctrl Pts',(3.56557511351408,-7.97608864298997,26.6868591278533));
#15875=CARTESIAN_POINT('Ctrl Pts',(3.56886142596211,-7.95633642607221,26.6864207157745));
#15876=CARTESIAN_POINT('Ctrl Pts',(3.57561990006005,-7.93776767109828,26.685515140808));
#15877=CARTESIAN_POINT('',(3.57561990006051,-7.93776767109862,25.8310328114859));
#15878=CARTESIAN_POINT('',(3.57561990005985,-7.93776767109862,53.8479999999999));
#15879=CARTESIAN_POINT('',(3.7321349388082,-8.16129431171214,25.8088837917547));
#15880=CARTESIAN_POINT('Ctrl Pts',(3.57561990006,-7.93776767109842,25.8310328114862));
#15881=CARTESIAN_POINT('Ctrl Pts',(3.56886152968978,-7.95633614108284,25.8319683282255));
#15882=CARTESIAN_POINT('Ctrl Pts',(3.56557511351408,-7.97609068679801,25.8324212548431));
#15883=CARTESIAN_POINT('Ctrl Pts',(3.56557511351408,-8.01569048646167,25.8324212548431));
#15884=CARTESIAN_POINT('Ctrl Pts',(3.56977332643641,-8.03802533272474,25.8318430858134));
#15885=CARTESIAN_POINT('Ctrl Pts',(3.58679186409018,-8.07906231912398,25.8294851140769));
#15886=CARTESIAN_POINT('Ctrl Pts',(3.5996132579237,-8.09776396941093,25.8277045026782));
#15887=CARTESIAN_POINT('Ctrl Pts',(3.62919326044957,-8.12734397193681,25.8235647115329));
#15888=CARTESIAN_POINT('Ctrl Pts',(3.6479545391554,-8.14016035449142,25.8209252662438));
#15889=CARTESIAN_POINT('Ctrl Pts',(3.68899328103869,-8.1571361600303,25.815093674543));
#15890=CARTESIAN_POINT('Ctrl Pts',(3.71127117091831,-8.16129431171213,25.8119008302958));
#15891=CARTESIAN_POINT('Ctrl Pts',(3.73213493880821,-8.16129431171213,25.8088837917549));
#15892=CARTESIAN_POINT('',(3.73213493880821,-8.16129431171214,53.8479999999997));
#15893=CARTESIAN_POINT('Origin',(-7.49147704148101,-8.35561410788639,27.4319999999996));
#15894=CARTESIAN_POINT('',(-7.49147704148201,-8.71649372935708,24.9780921111826));
#15895=CARTESIAN_POINT('',(-7.49147704148101,-8.71649372935708,27.4319999999996));
#15896=CARTESIAN_POINT('',(-7.83059295876998,-8.23218600802769,24.8738643497915));
#15897=CARTESIAN_POINT('Ctrl Pts',(-7.49147704148101,-8.71649372935708,
24.978092111183));
#15898=CARTESIAN_POINT('Ctrl Pts',(-7.53697327767576,-8.71649372935708,
24.9644467932216));
#15899=CARTESIAN_POINT('Ctrl Pts',(-7.5855872840004,-8.70738049023123,24.9497170260038));
#15900=CARTESIAN_POINT('Ctrl Pts',(-7.67529682874644,-8.66994929686166,
24.9222658021177));
#15901=CARTESIAN_POINT('Ctrl Pts',(-7.71639137271658,-8.64162338666943,
24.9095519450883));
#15902=CARTESIAN_POINT('Ctrl Pts',(-7.77987853657933,-8.57699837170364,
24.8897942019286));
#15903=CARTESIAN_POINT('Ctrl Pts',(-7.80707899432531,-8.53699031052272,
24.8812618711769));
#15904=CARTESIAN_POINT('Ctrl Pts',(-7.84332516491791,-8.44891371496679,
24.8698597720933));
#15905=CARTESIAN_POINT('Ctrl Pts',(-7.8523566629517,-8.40083772649981,24.8670024051066));
#15906=CARTESIAN_POINT('Ctrl Pts',(-7.8523566629517,-8.3150802474611,24.8670024051066));
#15907=CARTESIAN_POINT('Ctrl Pts',(-7.84518678820432,-8.27228222486467,
24.8692700360011));
#15908=CARTESIAN_POINT('Ctrl Pts',(-7.83059295876916,-8.23218600802805,
24.8738643497921));
#15909=CARTESIAN_POINT('',(-7.83059295876898,-8.23218600802769,27.4319999999994));
#15910=CARTESIAN_POINT('Origin',(-6.56755945719023,-7.99473448641546,27.4319999999997));
#15911=CARTESIAN_POINT('',(-6.7240744959397,-7.937767671096,25.1955181719057));
#15912=CARTESIAN_POINT('',(-6.7240744959387,-7.937767671096,27.4319999999997));
#15913=CARTESIAN_POINT('',(-6.56755945719123,-8.16129431170977,25.2367683460866));
#15914=CARTESIAN_POINT('Ctrl Pts',(-6.72407449593881,-7.93776767109636,
25.195518171906));
#15915=CARTESIAN_POINT('Ctrl Pts',(-6.73081874565397,-7.95629734490004,
25.1937182947535));
#15916=CARTESIAN_POINT('Ctrl Pts',(-6.73411928248454,-7.97605828905288,
25.1928353161579));
#15917=CARTESIAN_POINT('Ctrl Pts',(-6.73411928248454,-8.01561472817006,
25.1928353161579));
#15918=CARTESIAN_POINT('Ctrl Pts',(-6.72994693326961,-8.037832607282,25.193951956306));
#15919=CARTESIAN_POINT('Ctrl Pts',(-6.71315335554495,-8.07858586638705,
25.1984315097792));
#15920=CARTESIAN_POINT('Ctrl Pts',(-6.70052857822673,-8.0971197600608,25.2017946399685));
#15921=CARTESIAN_POINT('Ctrl Pts',(-6.67115094796283,-8.12688784587934,
25.2095874286932));
#15922=CARTESIAN_POINT('Ctrl Pts',(-6.6522374931881,-8.13989601918605,25.2145893678813));
#15923=CARTESIAN_POINT('Ctrl Pts',(-6.61092483986377,-8.15710113986306,
25.2254520703065));
#15924=CARTESIAN_POINT('Ctrl Pts',(-6.58852400246716,-8.16129431170978,
25.2313125802887));
#15925=CARTESIAN_POINT('Ctrl Pts',(-6.56755945719023,-8.16129431170978,
25.2367683460869));
#15926=CARTESIAN_POINT('',(-6.56755945719023,-8.16129431170977,27.4319999999997));
#15927=CARTESIAN_POINT('Origin',(-3.62500254366004,-7.99473448641784,53.8479999999997));
#15928=CARTESIAN_POINT('',(-3.78151758240752,-7.93776767109836,26.6571172630112));
#15929=CARTESIAN_POINT('',(-3.62500254365905,-8.16129431171214,26.6788517848586));
#15930=CARTESIAN_POINT('Ctrl Pts',(-3.62500254366004,-8.16129431171215,
26.6788517848587));
#15931=CARTESIAN_POINT('Ctrl Pts',(-3.64593323088655,-8.16129431171215,
26.6760078170955));
#15932=CARTESIAN_POINT('Ctrl Pts',(-3.66826838157995,-8.15710986236324,
26.6729451550951));
#15933=CARTESIAN_POINT('Ctrl Pts',(-3.70938341172565,-8.14005217200599,
26.6672588028701));
#15934=CARTESIAN_POINT('Ctrl Pts',(-3.72816376248556,-8.12717988138874,
26.6646356695417));
#15935=CARTESIAN_POINT('Ctrl Pts',(-3.7576812233659,-8.09755126686952,26.6604918865349));
#15936=CARTESIAN_POINT('Ctrl Pts',(-3.77044463206168,-8.07887773759886,
26.6586868787009));
#15937=CARTESIAN_POINT('Ctrl Pts',(-3.78738466317436,-8.03792135234649,
26.6562858956091));
#15938=CARTESIAN_POINT('Ctrl Pts',(-3.79156236895434,-8.01563891623561,
26.6556904019072));
#15939=CARTESIAN_POINT('Ctrl Pts',(-3.79156236895434,-7.9760899190566,26.6556904019072));
#15940=CARTESIAN_POINT('Ctrl Pts',(-3.78827575284781,-7.95633559177715,
26.656158564436));
#15941=CARTESIAN_POINT('Ctrl Pts',(-3.78151758240836,-7.93776767109807,
26.6571172630113));
#15942=CARTESIAN_POINT('',(-3.78151758240852,-7.93776767109836,25.8016944899306));
#15943=CARTESIAN_POINT('',(-3.78151758240851,-7.93776767109836,53.848));
#15944=CARTESIAN_POINT('',(-3.62500254365948,-8.16129431171214,25.8241489760309));
#15945=CARTESIAN_POINT('Ctrl Pts',(-3.78151758240848,-7.93776767109838,
25.8016944899306));
#15946=CARTESIAN_POINT('Ctrl Pts',(-3.78827538142984,-7.95633457131478,
25.8007040613436));
#15947=CARTESIAN_POINT('Ctrl Pts',(-3.79156236895434,-7.97608907531962,
25.8002203203793));
#15948=CARTESIAN_POINT('Ctrl Pts',(-3.79156236895434,-8.01563831096263,
25.8002203203793));
#15949=CARTESIAN_POINT('Ctrl Pts',(-3.78738478729748,-8.03791906403293,
25.8008355419363));
#15950=CARTESIAN_POINT('Ctrl Pts',(-3.77044862587136,-8.07887007028736,
25.8033155584679));
#15951=CARTESIAN_POINT('Ctrl Pts',(-3.75768889218056,-8.09753987582921,
25.8051798647189));
#15952=CARTESIAN_POINT('Ctrl Pts',(-3.72817533743971,-8.12717199367678,
25.8094604214847));
#15953=CARTESIAN_POINT('Ctrl Pts',(-3.70939159157236,-8.14004786848946,
25.8121709626822));
#15954=CARTESIAN_POINT('Ctrl Pts',(-3.66827136360832,-8.15710953514236,
25.8180463978047));
#15955=CARTESIAN_POINT('Ctrl Pts',(-3.6459343786089,-8.16129431171214,25.8212107202532));
#15956=CARTESIAN_POINT('Ctrl Pts',(-3.62500254366004,-8.16129431171214,
25.8241489760309));
#15957=CARTESIAN_POINT('',(-3.62500254366004,-8.16129431171214,53.8479999999997));
#15958=CARTESIAN_POINT('Origin',(-4.54892012795016,-8.35561410788639,27.432));
#15959=CARTESIAN_POINT('',(-4.54892012795116,-8.71649372935708,25.6775123298055));
#15960=CARTESIAN_POINT('',(-4.54892012795016,-8.71649372935708,27.432));
#15961=CARTESIAN_POINT('',(-4.88803604523924,-8.23218600802768,25.6151208741679));
#15962=CARTESIAN_POINT('Ctrl Pts',(-4.54892012795016,-8.71649372935709,
25.6775123298055));
#15963=CARTESIAN_POINT('Ctrl Pts',(-4.59431478588856,-8.71649372935709,
25.6694704030586));
#15964=CARTESIAN_POINT('Ctrl Pts',(-4.64275692379957,-8.70741149054491,
25.6607516981318));
#15965=CARTESIAN_POINT('Ctrl Pts',(-4.73196157379831,-8.67035617945831,
25.644451821608));
#15966=CARTESIAN_POINT('Ctrl Pts',(-4.77272412010716,-8.64238013938346,
25.6368775850129));
#15967=CARTESIAN_POINT('Ctrl Pts',(-4.83657480762835,-8.57810939638667,
25.6249076898685));
#15968=CARTESIAN_POINT('Ctrl Pts',(-4.86413692289329,-8.53774143998783,
25.6196766785593));
#15969=CARTESIAN_POINT('Ctrl Pts',(-4.9007519470913,-8.44913610232068,25.6126978561817));
#15970=CARTESIAN_POINT('Ctrl Pts',(-4.90979974942086,-8.4008959683684,25.6109582053926));
#15971=CARTESIAN_POINT('Ctrl Pts',(-4.90979974942086,-8.31518437158928,
25.6109582053926));
#15972=CARTESIAN_POINT('Ctrl Pts',(-4.90266825066707,-8.27238766204047,
25.6123286660847));
#15973=CARTESIAN_POINT('Ctrl Pts',(-4.88803604523831,-8.23218600802801,
25.6151208741679));
#15974=CARTESIAN_POINT('',(-4.88803604523824,-8.23218600802767,27.432));
#15975=CARTESIAN_POINT('Origin',(-0.134339559012431,-8.35561410788627,27.432));
#15976=CARTESIAN_POINT('',(-0.134339559012861,-8.71649372935708,26.0769873003126));
#15977=CARTESIAN_POINT('',(-0.134339559012431,-8.71649372935708,27.432));
#15978=CARTESIAN_POINT('',(-0.473455476301052,-8.23218600802749,26.0730349919173));
#15979=CARTESIAN_POINT('Ctrl Pts',(-0.134339559012431,-8.7164937293571,
26.0769873003126));
#15980=CARTESIAN_POINT('Ctrl Pts',(-0.179654315991581,-8.7164937293571,
26.0767538544625));
#15981=CARTESIAN_POINT('Ctrl Pts',(-0.227988401795148,-8.7074372467988,
26.0763745887362));
#15982=CARTESIAN_POINT('Ctrl Pts',(-0.316902065741546,-8.67060705694145,
26.0754456047097));
#15983=CARTESIAN_POINT('Ctrl Pts',(-0.357481735812576,-8.64283340165887,
26.0749026349481));
#15984=CARTESIAN_POINT('Ctrl Pts',(-0.421561871026094,-8.57875203541336,
26.0739453501203));
#15985=CARTESIAN_POINT('Ctrl Pts',(-0.449334423905883,-8.538173048106,26.0734683452426));
#15986=CARTESIAN_POINT('Ctrl Pts',(-0.486163107389859,-8.44926090347702,
26.0728076433653));
#15987=CARTESIAN_POINT('Ctrl Pts',(-0.495219180483252,-8.40092767225858,
26.0726307023488));
#15988=CARTESIAN_POINT('Ctrl Pts',(-0.495219180483254,-8.31524412923348,
26.0726307023488));
#15989=CARTESIAN_POINT('Ctrl Pts',(-0.48810997641732,-8.27244891619171,
26.0727688835285));
#15990=CARTESIAN_POINT('Ctrl Pts',(-0.473455476300624,-8.23218600802765,
26.0730349919173));
#15991=CARTESIAN_POINT('',(-0.473455476300511,-8.23218600802749,27.432));
#15992=CARTESIAN_POINT('Origin',(1.18682976815654,-6.90329429301814,27.432));
#15993=CARTESIAN_POINT('',(1.03031472940775,-6.84632747769874,26.0569715304013));
#15994=CARTESIAN_POINT('',(1.03031472940818,-6.84632747769874,27.432));
#15995=CARTESIAN_POINT('',(1.1636491207745,-7.06823316954214,26.0513576325976));
#15996=CARTESIAN_POINT('Ctrl Pts',(1.03031472940815,-6.84632747769889,26.0569715304013));
#15997=CARTESIAN_POINT('Ctrl Pts',(1.02355147137756,-6.86490937641994,26.0572389553536));
#15998=CARTESIAN_POINT('Ctrl Pts',(1.02026994286236,-6.88466130090506,26.0573667706749));
#15999=CARTESIAN_POINT('Ctrl Pts',(1.02026994286236,-6.92421148476832,26.0573667706749));
#16000=CARTESIAN_POINT('Ctrl Pts',(1.02445111149625,-6.94652146861111,26.0572043214501));
#16001=CARTESIAN_POINT('Ctrl Pts',(1.04145095426441,-6.9875584541026,26.0565300037632));
#16002=CARTESIAN_POINT('Ctrl Pts',(1.05426971905499,-7.00628540779412,26.0560175024064));
#16003=CARTESIAN_POINT('Ctrl Pts',(1.0838471911554,-7.03586287989453,26.0548039379574));
#16004=CARTESIAN_POINT('Ctrl Pts',(1.10258023978664,-7.04868134491983,26.0540220127177));
#16005=CARTESIAN_POINT('Ctrl Pts',(1.1361672091402,-7.06259140550485,26.0525738128797));
#16006=CARTESIAN_POINT('Ctrl Pts',(1.14995173485719,-7.06630812749198,26.0519694606376));
#16007=CARTESIAN_POINT('Ctrl Pts',(1.16364912077451,-7.06823316954208,26.0513576325976));
#16008=CARTESIAN_POINT('',(1.16364912077505,-7.06823316954214,27.432));
#16009=CARTESIAN_POINT('Origin',(0.339115917287747,-7.05480587763417,27.432));
#16010=CARTESIAN_POINT('',(0.288891181293952,-7.41217344343619,26.0757330800717));
#16011=CARTESIAN_POINT('',(0.288891181294382,-7.41217344343619,27.432));
#16012=CARTESIAN_POINT('',(-7.63278329429795E-13,-6.93137777777542,26.0773333333334));
#16013=CARTESIAN_POINT('Ctrl Pts',(0.288891181293958,-7.41217344343615,
26.0757330800718));
#16014=CARTESIAN_POINT('Ctrl Pts',(0.259205694102505,-7.40800142028769,
26.0760619634607));
#16015=CARTESIAN_POINT('Ctrl Pts',(0.229333439996986,-7.39994549874657,
26.0763402699514));
#16016=CARTESIAN_POINT('Ctrl Pts',(0.156559108768235,-7.36980209150743,
26.0769012645056));
#16017=CARTESIAN_POINT('Ctrl Pts',(0.115977788337335,-7.34202853546776,
26.0770951149185));
#16018=CARTESIAN_POINT('Ctrl Pts',(0.0518947122397707,-7.27794559593558,
26.0773013817785));
#16019=CARTESIAN_POINT('Ctrl Pts',(0.0241213296827975,-7.23736547331769,
26.0773286790822));
#16020=CARTESIAN_POINT('Ctrl Pts',(-0.0127078778804065,-7.14845209138881,
26.0773367387329));
#16021=CARTESIAN_POINT('Ctrl Pts',(-0.0217637041830148,-7.10011883335484,
26.0773242515209));
#16022=CARTESIAN_POINT('Ctrl Pts',(-0.0217637041830148,-7.01443642362561,
26.0773242515209));
#16023=CARTESIAN_POINT('Ctrl Pts',(-0.0146546813736372,-6.97164118393791,
26.0773333333334));
#16024=CARTESIAN_POINT('Ctrl Pts',(-3.87466119286765E-13,-6.93137777777556,
26.0773333333334));
#16025=CARTESIAN_POINT('',(-3.33066907387547E-13,-6.93137777777542,27.432));
#16026=CARTESIAN_POINT('Origin',(0.789578025278126,-7.99473448641556,27.432));
#16027=CARTESIAN_POINT('',(0.633062986529334,-7.9377676710961,26.0696479652653));
#16028=CARTESIAN_POINT('',(0.633062986529875,-7.9377676710961,27.432));
#16029=CARTESIAN_POINT('',(0.789578025277696,-8.16129431170975,26.065377041581));
#16030=CARTESIAN_POINT('Ctrl Pts',(0.633062986529732,-7.93776767109625,
26.0696479652654));
#16031=CARTESIAN_POINT('Ctrl Pts',(0.626299463794731,-7.95635029708667,
26.0698122074488));
#16032=CARTESIAN_POINT('Ctrl Pts',(0.62301819998392,-7.97610197906074,26.0698899518251));
#16033=CARTESIAN_POINT('Ctrl Pts',(0.623018199983922,-8.01564751192798,
26.0698899518251));
#16034=CARTESIAN_POINT('Ctrl Pts',(0.627197620279825,-8.03795408858184,
26.0697913331208));
#16035=CARTESIAN_POINT('Ctrl Pts',(0.644193422212709,-8.07898802424257,
26.0693764918328));
#16036=CARTESIAN_POINT('Ctrl Pts',(0.657009838816212,-8.0977153624133,26.0690596410441));
#16037=CARTESIAN_POINT('Ctrl Pts',(0.686584805954723,-8.12729453212123,
26.0682974893448));
#16038=CARTESIAN_POINT('Ctrl Pts',(0.705316964028781,-8.1401152284569,26.0678014763646));
#16039=CARTESIAN_POINT('Ctrl Pts',(0.7463572594525,-8.15711515419391,26.0666583110525));
#16040=CARTESIAN_POINT('Ctrl Pts',(0.768665409093284,-8.16129431170976,
26.0660105310627));
#16041=CARTESIAN_POINT('Ctrl Pts',(0.789578025278126,-8.16129431170976,
26.065377041581));
#16042=CARTESIAN_POINT('',(0.789578025278126,-8.16129431170977,27.432));
#16043=CARTESIAN_POINT('Origin',(0.,-73.5076,0.));
#16044=CARTESIAN_POINT('',(-1.33755923402874E-15,0.,10.922));
#16045=CARTESIAN_POINT('Origin',(0.,0.,0.));
#16046=CARTESIAN_POINT('',(-1.33755923402874E-15,-2.54,10.922));
#16047=CARTESIAN_POINT('',(-1.33755923402874E-15,-73.5076,10.922));
#16048=CARTESIAN_POINT('Origin',(0.,-2.54,0.));
#16049=CARTESIAN_POINT('Origin',(0.,-5.715,0.));
#16050=CARTESIAN_POINT('',(17.7836282012407,-2.54,11.5569999999998));
#16051=CARTESIAN_POINT('',(17.7836282012417,-2.54,-11.5570000000003));
#16052=CARTESIAN_POINT('Origin',(0.,-2.54,0.));
#16053=CARTESIAN_POINT('',(19.4305849628867,-5.715,14.7319999999999));
#16054=CARTESIAN_POINT('Ctrl Pts',(17.7836282012417,-2.54,11.557));
#16055=CARTESIAN_POINT('Ctrl Pts',(17.7850716643977,-2.54,11.5596595536768));
#16056=CARTESIAN_POINT('Ctrl Pts',(17.7865149917423,-2.54000334168149,11.5623191809317));
#16057=CARTESIAN_POINT('Ctrl Pts',(17.9248879627353,-2.54064419609321,11.8173308490795));
#16058=CARTESIAN_POINT('Ctrl Pts',(18.0604631387315,-2.57136469893144,12.0701380075818));
#16059=CARTESIAN_POINT('Ctrl Pts',(18.3213429812865,-2.69274046261169,12.561839726354));
#16060=CARTESIAN_POINT('Ctrl Pts',(18.4465074467427,-2.78234246612,12.8003808929793));
#16061=CARTESIAN_POINT('Ctrl Pts',(18.7478882421779,-3.08534809936439,13.3800594828894));
#16062=CARTESIAN_POINT('Ctrl Pts',(18.9127794136079,-3.33811416464457,13.7025220477582));
#16063=CARTESIAN_POINT('Ctrl Pts',(19.1719691929213,-3.93743554810769,14.2140617953081));
#16064=CARTESIAN_POINT('Ctrl Pts',(19.2694863540614,-4.26683227457329,14.4088092531595));
#16065=CARTESIAN_POINT('Ctrl Pts',(19.3980919281663,-4.9753874034505,14.6664389763375));
#16066=CARTESIAN_POINT('Ctrl Pts',(19.4305849628878,-5.34244154426032,14.732));
#16067=CARTESIAN_POINT('Ctrl Pts',(19.4305849628878,-5.715,14.732));
#16068=CARTESIAN_POINT('',(19.4305849628877,-5.715,-14.7320000000001));
#16069=CARTESIAN_POINT('Origin',(0.,-5.715,0.));
#16070=CARTESIAN_POINT('Ctrl Pts',(19.4305849628878,-5.715,-14.732));
#16071=CARTESIAN_POINT('Ctrl Pts',(19.4305849628878,-5.34244154426032,-14.732));
#16072=CARTESIAN_POINT('Ctrl Pts',(19.3980919281663,-4.9753874034505,-14.6664389763376));
#16073=CARTESIAN_POINT('Ctrl Pts',(19.2694863540614,-4.26683227457328,-14.4088092531595));
#16074=CARTESIAN_POINT('Ctrl Pts',(19.1719691929212,-3.93743554810768,-14.2140617953081));
#16075=CARTESIAN_POINT('Ctrl Pts',(18.9127794136079,-3.33811416464457,-13.7025220477582));
#16076=CARTESIAN_POINT('Ctrl Pts',(18.7478882421779,-3.0853480993644,-13.3800594828895));
#16077=CARTESIAN_POINT('Ctrl Pts',(18.4465074467427,-2.78234246612,-12.8003808929793));
#16078=CARTESIAN_POINT('Ctrl Pts',(18.3213429812865,-2.69274046261169,-12.561839726354));
#16079=CARTESIAN_POINT('Ctrl Pts',(18.0604631387314,-2.57136469893143,-12.0701380075818));
#16080=CARTESIAN_POINT('Ctrl Pts',(17.9248879627351,-2.54064419609321,-11.8173308490792));
#16081=CARTESIAN_POINT('Ctrl Pts',(17.7865149917423,-2.54000334168149,-11.5623191809317));
#16082=CARTESIAN_POINT('Ctrl Pts',(17.7850716643978,-2.54,-11.559659553677));
#16083=CARTESIAN_POINT('Ctrl Pts',(17.7836282012418,-2.54,-11.5570000000002));
#16084=CARTESIAN_POINT('Origin',(0.,-73.5076,0.));
#16085=CARTESIAN_POINT('',(19.4305849628866,-61.0824288944265,14.7319999999999));
#16086=CARTESIAN_POINT('',(19.4305849628866,-73.5076,14.7319999999999));
#16087=CARTESIAN_POINT('',(19.4305849628877,-61.0824288944265,-14.7320000000001));
#16088=CARTESIAN_POINT('Origin',(-3.3318285429356E-14,-39.4709528472727,
0.));
#16089=CARTESIAN_POINT('',(19.4305849628877,-73.5076,-14.7320000000001));
#16090=CARTESIAN_POINT('Origin',(35.5599999999999,-62.3824,38.0999999999997));
#16091=CARTESIAN_POINT('',(32.3151499999999,-62.3824,-17.2720000000001));
#16092=CARTESIAN_POINT('Origin',(35.5599999999989,-62.3824,-17.2720000000001));
#16093=CARTESIAN_POINT('',(32.3151499999999,-62.3824,-14.7320000000001));
#16094=CARTESIAN_POINT('',(32.3151499999999,-62.3824,38.0999999999997));
#16095=CARTESIAN_POINT('Origin',(35.5599999999999,-62.3824,-14.7320000000001));
#16096=CARTESIAN_POINT('Origin',(35.5599999999999,-62.3824,38.0999999999997));
#16097=CARTESIAN_POINT('',(31.5277499999999,-62.3824,14.7319999999999));
#16098=CARTESIAN_POINT('Origin',(35.5599999999989,-62.3824,14.7319999999999));
#16099=CARTESIAN_POINT('',(31.5277499999999,-62.3824,17.2719999999999));
#16100=CARTESIAN_POINT('',(31.5277499999999,-62.3824,38.0999999999997));
#16101=CARTESIAN_POINT('Origin',(35.5599999999999,-62.3824,17.2719999999999));
#16102=CARTESIAN_POINT('Origin',(-26.9240000000011,-9.525,32.3088));
#16103=CARTESIAN_POINT('',(27.2869469125796,-69.8205898102122,-17.272));
#16104=CARTESIAN_POINT('',(38.7859348280757,-82.6102254478887,-17.2720000000002));
#16105=CARTESIAN_POINT('',(27.2869469125807,-69.8205898102122,-14.732));
#16106=CARTESIAN_POINT('',(27.2869469125796,-69.8205898102122,32.3088));
#16107=CARTESIAN_POINT('',(38.7859348280768,-82.6102254478887,-14.7320000000002));
#16108=CARTESIAN_POINT('',(27.2869469125796,-69.8205898102122,14.732));
#16109=CARTESIAN_POINT('',(5.08051787432773,-45.1217086303799,14.732));
#16110=CARTESIAN_POINT('',(27.2869469125807,-69.8205898102122,17.272));
#16111=CARTESIAN_POINT('',(27.2869469125796,-69.8205898102122,32.3088));
#16112=CARTESIAN_POINT('',(3.81766973068887,-43.717118266292,17.2719999999997));
#16113=CARTESIAN_POINT('Origin',(46.6851999999989,-62.3824,32.3088));
#16114=CARTESIAN_POINT('',(46.6852,-62.3824,17.272));
#16115=CARTESIAN_POINT('',(46.685199999999,-62.3824,14.732));
#16116=CARTESIAN_POINT('',(46.6851999999989,-62.3824,32.3088));
#16117=CARTESIAN_POINT('',(28.2728456056904,-5.715,14.7319999999997));
#16118=CARTESIAN_POINT('',(30.2435414105375,-11.780178035359,14.7319999999999));
#16119=CARTESIAN_POINT('',(27.2412255701507,-2.54,11.557));
#16120=CARTESIAN_POINT('Origin',(28.2728456056901,-5.71499999999969,11.5570000000002));
#16121=CARTESIAN_POINT('',(27.2412255701519,-2.54,-11.557));
#16122=CARTESIAN_POINT('',(27.2412255701519,-2.54,-11.557));
#16123=CARTESIAN_POINT('',(28.2728456056914,-5.715,-14.7320000000002));
#16124=CARTESIAN_POINT('Origin',(28.2728456056913,-5.71499999999997,-11.5570000000002));
#16125=CARTESIAN_POINT('',(46.6852,-62.3824,-14.732));
#16126=CARTESIAN_POINT('',(50.1672866578201,-73.0991607817904,-14.732));
#16127=CARTESIAN_POINT('',(46.685199999999,-62.3824,-17.272));
#16128=CARTESIAN_POINT('',(46.6851999999989,-62.3824,32.3088));
#16129=CARTESIAN_POINT('',(27.4475495772589,-3.175,-17.272));
#16130=CARTESIAN_POINT('',(50.167286657819,-73.0991607817904,-17.272));
#16131=CARTESIAN_POINT('',(26.4159295417202,0.,-14.097));
#16132=CARTESIAN_POINT('Origin',(27.4475495772584,-3.1750000000003,-14.0970000000001));
#16133=CARTESIAN_POINT('',(26.4159295417197,0.,14.097));
#16134=CARTESIAN_POINT('',(26.4159295417192,0.,32.3088));
#16135=CARTESIAN_POINT('',(27.4475495772599,-3.175,17.272));
#16136=CARTESIAN_POINT('Origin',(27.4475495772597,-3.17499999999968,14.0970000000002));
#16137=CARTESIAN_POINT('',(29.4970541401273,-9.48272645250279,17.2719999999996));
#16138=CARTESIAN_POINT('Origin',(35.5599999999989,-62.3824,32.3087999999997));
#16139=CARTESIAN_POINT('Origin',(35.5599999999999,-62.3824,-14.7320000000001));
#16140=CARTESIAN_POINT('Origin',(35.5599999999989,-62.3824,-17.2720000000001));
#16141=CARTESIAN_POINT('Origin',(35.5599999999989,-62.3824,32.3087999999997));
#16142=CARTESIAN_POINT('Origin',(35.5599999999989,-62.3824,14.7319999999999));
#16143=CARTESIAN_POINT('Origin',(35.5599999999999,-62.3824,17.2719999999999));
#16144=CARTESIAN_POINT('Origin',(48.91024,-2.54,-11.557));
#16145=CARTESIAN_POINT('',(48.9102399999989,-2.54,11.557));
#16146=CARTESIAN_POINT('',(48.91024,-2.54,-11.557));
#16147=CARTESIAN_POINT('Origin',(48.91024,-5.715,-11.557));
#16148=CARTESIAN_POINT('',(48.91024,-5.715,-14.732));
#16149=CARTESIAN_POINT('Origin',(48.9102399999989,-5.715,11.557));
#16150=CARTESIAN_POINT('',(48.9102399999989,-5.715,14.732));
#16151=CARTESIAN_POINT('Origin',(48.91024,-3.175,-14.097));
#16152=CARTESIAN_POINT('',(48.91024,0.,-14.097));
#16153=CARTESIAN_POINT('',(48.9102399999989,-3.175,-17.272));
#16154=CARTESIAN_POINT('Origin',(48.9102399999989,-3.175,14.097));
#16155=CARTESIAN_POINT('',(48.91024,-3.175,17.272));
#16156=CARTESIAN_POINT('',(48.9102399999989,0.,14.097));
#16157=CARTESIAN_POINT('Origin',(48.9102399999989,-73.5076,-17.272));
#16158=CARTESIAN_POINT('Origin',(48.91024,-3.175,17.272));
#16159=CARTESIAN_POINT('Origin',(0.,0.,0.));
#16160=CARTESIAN_POINT('Origin',(0.934758973429761,-7.99473448641561,27.432));
#16161=CARTESIAN_POINT('',(0.93475897342922,-8.16129431170975,26.0605744265043));
#16162=CARTESIAN_POINT('',(0.934758973429761,-8.16129431170977,27.432));
#16163=CARTESIAN_POINT('',(1.09127401217758,-8.05170130173499,26.0544897245777));
#16164=CARTESIAN_POINT('Ctrl Pts',(1.09127401217801,-8.05170130173515,26.0544897245777));
#16165=CARTESIAN_POINT('Ctrl Pts',(1.08828433996508,-8.05991535863171,26.0546149448996));
#16166=CARTESIAN_POINT('Ctrl Pts',(1.08462402696936,-8.06794736482996,26.0547683476573));
#16167=CARTESIAN_POINT('Ctrl Pts',(1.08034816426209,-8.07564161165686,26.0549456802091));
#16168=CARTESIAN_POINT('Ctrl Pts',(1.07607197682462,-8.083336442823,26.0551230262285));
#16169=CARTESIAN_POINT('Ctrl Pts',(1.07118066823125,-8.0906924967541,26.055324305677));
#16170=CARTESIAN_POINT('Ctrl Pts',(1.06577502913247,-8.09757887639445,26.055545264944));
#16171=CARTESIAN_POINT('Ctrl Pts',(1.06505888750446,-8.09849118723072,26.0555745377323));
#16172=CARTESIAN_POINT('Ctrl Pts',(1.06433377689196,-8.09939530225319,26.0556041559227));
#16173=CARTESIAN_POINT('Ctrl Pts',(1.06359998267504,-8.10029096295151,26.0556341096246));
#16174=CARTESIAN_POINT('Ctrl Pts',(1.05805747246737,-8.107056086536,26.0558603565681));
#16175=CARTESIAN_POINT('Ctrl Pts',(1.05194190694434,-8.11342692481915,26.0561085689308));
#16176=CARTESIAN_POINT('Ctrl Pts',(1.0453568909017,-8.11927474517913,26.0563727655387));
#16177=CARTESIAN_POINT('Ctrl Pts',(1.03877138132252,-8.12512300382401,26.0566369819477));
#16178=CARTESIAN_POINT('Ctrl Pts',(1.03171716354121,-8.13044742703919,26.056917184998));
#16179=CARTESIAN_POINT('Ctrl Pts',(1.02433274661679,-8.13515782692229,26.0572073921708));
#16180=CARTESIAN_POINT('Ctrl Pts',(1.02336658586311,-8.13577412520931,26.0572453622344));
#16181=CARTESIAN_POINT('Ctrl Pts',(1.02239481070753,-8.13637997479871,26.0572835035539));
#16182=CARTESIAN_POINT('Ctrl Pts',(1.02141776309065,-8.13697523155049,26.0573218027299));
#16183=CARTESIAN_POINT('Ctrl Pts',(1.01345714013773,-8.14182516361034,26.0576338502638));
#16184=CARTESIAN_POINT('Ctrl Pts',(1.00503009397575,-8.14603688612667,26.0579605724836));
#16185=CARTESIAN_POINT('Ctrl Pts',(0.996299646991391,-8.1495082597094,26.0582943533982));
#16186=CARTESIAN_POINT('Ctrl Pts',(0.987569200007038,-8.15297963329213,
26.0586281343128));
#16187=CARTESIAN_POINT('Ctrl Pts',(0.97853660437262,-8.15571012256495,26.0589689739223));
#16188=CARTESIAN_POINT('Ctrl Pts',(0.969388912998919,-8.15765453640165,
26.0593092562358));
#16189=CARTESIAN_POINT('Ctrl Pts',(0.961424934126287,-8.15934734282488,
26.0596055059719));
#16190=CARTESIAN_POINT('Ctrl Pts',(0.953274387229974,-8.16046502621771,
26.059904974342));
#16191=CARTESIAN_POINT('Ctrl Pts',(0.94508914072775,-8.1609736606364,26.0602018306534));
#16192=CARTESIAN_POINT('Ctrl Pts',(0.941647888163826,-8.16118750141651,
26.0603266353911));
#16193=CARTESIAN_POINT('Ctrl Pts',(0.93820063876226,-8.16129431170977,26.0604509784367));
#16194=CARTESIAN_POINT('Ctrl Pts',(0.93475897342922,-8.16129431170975,26.0605744265043));
#16195=CARTESIAN_POINT('',(1.09127401217801,-8.05170130173499,27.432));
#16196=CARTESIAN_POINT('Origin',(0.934758973429761,-8.16129431170977,27.432));
#16197=CARTESIAN_POINT('Origin',(0.,-8.16129431170974,0.));
#16198=CARTESIAN_POINT('Origin',(1.04680588997652,-7.68688811328358,27.432));
#16199=CARTESIAN_POINT('',(1.20332092872445,-7.74385492860298,26.0495553228893));
#16200=CARTESIAN_POINT('',(1.20332092872488,-7.74385492860298,27.432));
#16201=CARTESIAN_POINT('',(1.06998653735758,-7.52194923675958,26.0553726242334));
#16202=CARTESIAN_POINT('Ctrl Pts',(1.06998653735759,-7.5219492367595,26.0553726242334));
#16203=CARTESIAN_POINT('Ctrl Pts',(1.07865102525531,-7.52316695112089,26.0550168095023));
#16204=CARTESIAN_POINT('Ctrl Pts',(1.08727712504398,-7.52507987610552,26.0546581952066));
#16205=CARTESIAN_POINT('Ctrl Pts',(1.09570086529067,-7.52766670520332,26.0543039582946));
#16206=CARTESIAN_POINT('Ctrl Pts',(1.10412492879106,-7.53025363356844,26.0539497077891));
#16207=CARTESIAN_POINT('Ctrl Pts',(1.11234556277567,-7.5335142099328,26.0535998350032));
#16208=CARTESIAN_POINT('Ctrl Pts',(1.12021350111099,-7.53737725070309,26.0532615177115));
#16209=CARTESIAN_POINT('Ctrl Pts',(1.12125071733421,-7.53788650845107,26.0532169179487));
#16210=CARTESIAN_POINT('Ctrl Pts',(1.12228183810229,-7.53840617015228,26.0531725190051));
#16211=CARTESIAN_POINT('Ctrl Pts',(1.12330655506529,-7.53893601413319,26.053128337325));
#16212=CARTESIAN_POINT('Ctrl Pts',(1.1310755525176,-7.54295308097839,26.0527933693556));
#16213=CARTESIAN_POINT('Ctrl Pts',(1.13857871012851,-7.54761310663511,26.0524666406882));
#16214=CARTESIAN_POINT('Ctrl Pts',(1.1456683226876,-7.55284187200663,26.0521549126148));
#16215=CARTESIAN_POINT('Ctrl Pts',(1.15275807009356,-7.55807073683106,26.0518431786121));
#16216=CARTESIAN_POINT('Ctrl Pts',(1.15943336297434,-7.56386772441556,26.051546445774));
#16217=CARTESIAN_POINT('Ctrl Pts',(1.16557685185692,-7.57011639574875,26.0512714757779));
#16218=CARTESIAN_POINT('Ctrl Pts',(1.16639367747828,-7.57094720621198,26.0512349163339));
#16219=CARTESIAN_POINT('Ctrl Pts',(1.16720115671943,-7.57178594941401,26.0511987416093));
#16220=CARTESIAN_POINT('Ctrl Pts',(1.16799906622218,-7.57263230628228,26.0511629674969));
#16221=CARTESIAN_POINT('Ctrl Pts',(1.17399436724834,-7.57899162921718,26.0508941693788));
#16222=CARTESIAN_POINT('Ctrl Pts',(1.17952673825722,-7.58586905066624,26.0506446154929));
#16223=CARTESIAN_POINT('Ctrl Pts',(1.18448140156036,-7.5931457593972,26.0504193973555));
#16224=CARTESIAN_POINT('Ctrl Pts',(1.18943613076021,-7.60042256490792,26.0501941762227));
#16225=CARTESIAN_POINT('Ctrl Pts',(1.19381250465264,-7.6080977700653,26.0499932914856));
#16226=CARTESIAN_POINT('Ctrl Pts',(1.1975383607578,-7.61602276452834,26.0498218348637));
#16227=CARTESIAN_POINT('Ctrl Pts',(1.19803800275604,-7.61708551627123,26.0497988423147));
#16228=CARTESIAN_POINT('Ctrl Pts',(1.19852601644932,-7.61815272848248,26.0497763789758));
#16229=CARTESIAN_POINT('Ctrl Pts',(1.1990022940857,-7.61922401661284,26.049754457126));
#16230=CARTESIAN_POINT('Ctrl Pts',(1.20255056563794,-7.62720512029448,26.0495911392));
#16231=CARTESIAN_POINT('Ctrl Pts',(1.20549117264442,-7.63552127348075,26.0494558415912));
#16232=CARTESIAN_POINT('Ctrl Pts',(1.20775528594202,-7.64402242373619,26.0493509408305));
#16233=CARTESIAN_POINT('Ctrl Pts',(1.21001946068967,-7.65252380472045,26.0492460372228));
#16234=CARTESIAN_POINT('Ctrl Pts',(1.21160680665617,-7.66120913563562,26.0491715321133));
#16235=CARTESIAN_POINT('Ctrl Pts',(1.21249858128217,-7.66991438505669,26.0491298022266));
#16236=CARTESIAN_POINT('Ctrl Pts',(1.21261805799343,-7.67108068261789,26.0491242114086));
#16237=CARTESIAN_POINT('Ctrl Pts',(1.21272512583901,-7.67224733122013,26.0491192088948));
#16238=CARTESIAN_POINT('Ctrl Pts',(1.21281981073847,-7.67341393370641,26.0491148004008));
#16239=CARTESIAN_POINT('Ctrl Pts',(1.21357321870269,-7.68269659239132,26.049079722004));
#16240=CARTESIAN_POINT('Ctrl Pts',(1.21354825442906,-7.69210957745951,26.0490817890873));
#16241=CARTESIAN_POINT('Ctrl Pts',(1.21272706430119,-7.70145998045125,26.0491200511282));
#16242=CARTESIAN_POINT('Ctrl Pts',(1.21190587417332,-7.710810383443,26.049158313169));
#16243=CARTESIAN_POINT('Ctrl Pts',(1.21028854984413,-7.7200968162067,26.0492327701674));
#16244=CARTESIAN_POINT('Ctrl Pts',(1.20791992919952,-7.72913076669552,26.0493424716008));
#16245=CARTESIAN_POINT('Ctrl Pts',(1.20662481586703,-7.73407034608732,26.0494024541013));
#16246=CARTESIAN_POINT('Ctrl Pts',(1.20508556703815,-7.73900662468374,26.0494738080156));
#16247=CARTESIAN_POINT('Ctrl Pts',(1.20332092872482,-7.74385492860311,26.0495553228893));
#16248=CARTESIAN_POINT('',(1.06998653735801,-7.52194923675958,27.432));
#16249=CARTESIAN_POINT('Origin',(1.20332092872488,-7.74385492860298,27.432));
#16250=CARTESIAN_POINT('Origin',(0.000220107120595808,-11.0493468518379,
0.00496806684324724));
#16251=CARTESIAN_POINT('Origin',(0.613341870778106,-6.30137626259121,27.432));
#16252=CARTESIAN_POINT('',(0.613341870777676,-5.94049664112042,26.0701193999439));
#16253=CARTESIAN_POINT('',(0.613341870778106,-5.94049664112042,27.432));
#16254=CARTESIAN_POINT('',(0.274225953489596,-6.17794816273243,26.0758914306724));
#16255=CARTESIAN_POINT('',(0.274225953490026,-6.17794816273243,27.432));
#16256=CARTESIAN_POINT('Ctrl Pts',(0.274225953489962,-6.17794816273256,
26.0758914306724));
#16257=CARTESIAN_POINT('Ctrl Pts',(0.276020658192973,-6.17301725208644,
26.0758725567401));
#16258=CARTESIAN_POINT('Ctrl Pts',(0.277924007236334,-6.16812266360616,
26.0758523554098));
#16259=CARTESIAN_POINT('Ctrl Pts',(0.298347946782827,-6.11881549966047,
26.0756330972809));
#16260=CARTESIAN_POINT('Ctrl Pts',(0.326121404075587,-6.07823587422568,
26.0753137155698));
#16261=CARTESIAN_POINT('Ctrl Pts',(0.390205719924242,-6.01415155837703,
26.0744334608314));
#16262=CARTESIAN_POINT('Ctrl Pts',(0.430789151643105,-5.98637765402624,
26.0738127552276));
#16263=CARTESIAN_POINT('Ctrl Pts',(0.519703793895466,-5.94955026980533,
26.0721920607849));
#16264=CARTESIAN_POINT('Ctrl Pts',(0.568034819625911,-5.94049664112043,
26.0711853218558));
#16265=CARTESIAN_POINT('Ctrl Pts',(0.613341870778106,-5.94049664112043,
26.0701193999439));
#16266=CARTESIAN_POINT('Origin',(2.34365910677381,-6.30137626259108,27.432));
#16267=CARTESIAN_POINT('',(2.68277502406135,-6.42480436244983,25.9389674418243));
#16268=CARTESIAN_POINT('',(2.68277502406178,-6.42480436244983,27.4319999999994));
#16269=CARTESIAN_POINT('',(2.34365910677338,-5.9404966411204,25.9718034754812));
#16270=CARTESIAN_POINT('',(2.34365910677381,-5.9404966411204,27.432));
#16271=CARTESIAN_POINT('Ctrl Pts',(2.34365910677381,-5.94049664112041,25.9718034754812));
#16272=CARTESIAN_POINT('Ctrl Pts',(2.38894892112891,-5.94049664112036,25.9677165861761));
#16273=CARTESIAN_POINT('Ctrl Pts',(2.43726044269616,-5.94954132393131,25.9632253297812));
#16274=CARTESIAN_POINT('Ctrl Pts',(2.52616829296165,-5.98635335706567,25.9547256149275));
#16275=CARTESIAN_POINT('Ctrl Pts',(2.56676501362077,-6.01412131437014,25.9507238865837));
#16276=CARTESIAN_POINT('Ctrl Pts',(2.63083501020314,-6.07819131095251,25.9443067917942));
#16277=CARTESIAN_POINT('Ctrl Pts',(2.65860971162163,-6.11873989244555,25.9414620120765));
#16278=CARTESIAN_POINT('Ctrl Pts',(2.69546232654362,-6.20765101794717,25.9376587179558));
#16279=CARTESIAN_POINT('Ctrl Pts',(2.70453872824448,-6.25601449073703,25.9367072706851));
#16280=CARTESIAN_POINT('Ctrl Pts',(2.70453872824448,-6.30137626259109,25.9367072706851));
#16281=CARTESIAN_POINT('Ctrl Pts',(2.70453872824448,-6.34176033266817,25.9367072706851));
#16282=CARTESIAN_POINT('Ctrl Pts',(2.69742339380224,-6.38455829735622,25.937452413111));
#16283=CARTESIAN_POINT('Ctrl Pts',(2.68277502406175,-6.42480436244995,25.9389674418249));
#16284=CARTESIAN_POINT('Origin',(1.41974152248314,-6.66225588406189,27.432));
#16285=CARTESIAN_POINT('',(1.57625656123096,-6.71922269938127,26.0296509586844));
#16286=CARTESIAN_POINT('',(1.57625656123139,-6.71922269938127,27.4319999999998));
#16287=CARTESIAN_POINT('',(1.41974152248271,-6.49569605876776,26.0386567969071));
#16288=CARTESIAN_POINT('Ctrl Pts',(1.41974152248271,-6.49569605876777,26.0386567969071));
#16289=CARTESIAN_POINT('Ctrl Pts',(1.42849740378437,-6.49569605876774,26.0381793879399));
#16290=CARTESIAN_POINT('Ctrl Pts',(1.43731182807135,-6.49639083046601,26.0376942319109));
#16291=CARTESIAN_POINT('Ctrl Pts',(1.4460193437173,-6.49778202135661,26.0372106626587));
#16292=CARTESIAN_POINT('Ctrl Pts',(1.45472723360787,-6.4991732720399,26.036727072623));
#16293=CARTESIAN_POINT('Ctrl Pts',(1.46332711870519,-6.50126084330025,26.0362450695004));
#16294=CARTESIAN_POINT('Ctrl Pts',(1.47166118278821,-6.50399494675955,26.0357739883332));
#16295=CARTESIAN_POINT('Ctrl Pts',(1.47275993535262,-6.50435540753323,26.0357118815825));
#16296=CARTESIAN_POINT('Ctrl Pts',(1.47385409198962,-6.50472703581456,26.0356499646712));
#16297=CARTESIAN_POINT('Ctrl Pts',(1.47494331621976,-6.50510965480306,26.0355882589912));
#16298=CARTESIAN_POINT('Ctrl Pts',(1.48320003098132,-6.50801004552423,26.0351205075536));
#16299=CARTESIAN_POINT('Ctrl Pts',(1.4912826784312,-6.51158491865049,26.0346589052539));
#16300=CARTESIAN_POINT('Ctrl Pts',(1.49903454603547,-6.51578134081994,26.0342126050108));
#16301=CARTESIAN_POINT('Ctrl Pts',(1.50678645238855,-6.51997778396579,26.0337663025369));
#16302=CARTESIAN_POINT('Ctrl Pts',(1.51420660147466,-6.52479527482055,26.0333353022726));
#16303=CARTESIAN_POINT('Ctrl Pts',(1.52116245354052,-6.53013484052429,26.032928757274));
#16304=CARTESIAN_POINT('Ctrl Pts',(1.52208873862297,-6.53084589073228,26.0328746191808));
#16305=CARTESIAN_POINT('Ctrl Pts',(1.52300683730169,-6.53156613967437,26.0328209147592));
#16306=CARTESIAN_POINT('Ctrl Pts',(1.52391648242519,-6.53229530110274,26.032767665624));
#16307=CARTESIAN_POINT('Ctrl Pts',(1.53073730155825,-6.53776279396696,26.0323683860471));
#16308=CARTESIAN_POINT('Ctrl Pts',(1.53717170672106,-6.54380810550216,26.0319896406627));
#16309=CARTESIAN_POINT('Ctrl Pts',(1.54308936433927,-6.55032963463199,26.0316389323484));
#16310=CARTESIAN_POINT('Ctrl Pts',(1.54900693448434,-6.55685106736242,26.0312882292181));
#16311=CARTESIAN_POINT('Ctrl Pts',(1.55440702041379,-6.5638479029416,26.0309655623289));
#16312=CARTESIAN_POINT('Ctrl Pts',(1.55919731721428,-6.57118307408044,26.0306784342258));
#16313=CARTESIAN_POINT('Ctrl Pts',(1.55984501729623,-6.57217486877411,26.0306396113921));
#16314=CARTESIAN_POINT('Ctrl Pts',(1.56048163523183,-6.57317280720191,26.0306014382775));
#16315=CARTESIAN_POINT('Ctrl Pts',(1.56110700642117,-6.57417651444008,26.0305639334278));
#16316=CARTESIAN_POINT('Ctrl Pts',(1.56572410332667,-6.58158685515025,26.0302870362367));
#16317=CARTESIAN_POINT('Ctrl Pts',(1.56978652751415,-6.58941338035424,26.0300430795855));
#16318=CARTESIAN_POINT('Ctrl Pts',(1.57320512254724,-6.59751718730813,26.0298365564472));
#16319=CARTESIAN_POINT('Ctrl Pts',(1.57662370788625,-6.60562097128213,26.0296300338946));
#16320=CARTESIAN_POINT('Ctrl Pts',(1.57939802408283,-6.61400103057099,26.0294609446427));
#16321=CARTESIAN_POINT('Ctrl Pts',(1.58148655577214,-6.62249761940721,26.0293337816265));
#16322=CARTESIAN_POINT('Ctrl Pts',(1.58176983603085,-6.62365006344049,26.029316533733));
#16323=CARTESIAN_POINT('Ctrl Pts',(1.58204057638361,-6.62480463373337,26.0293000571627));
#16324=CARTESIAN_POINT('Ctrl Pts',(1.58229874589317,-6.62596091858135,26.0292843631267));
#16325=CARTESIAN_POINT('Ctrl Pts',(1.58432780105419,-6.63504861349315,26.0291610175595));
#16326=CARTESIAN_POINT('Ctrl Pts',(1.58560440418134,-6.64437351947301,26.0290843603582));
#16327=CARTESIAN_POINT('Ctrl Pts',(1.58608388237221,-6.65374737605256,26.0290551943661));
#16328=CARTESIAN_POINT('Ctrl Pts',(1.58656336056309,-6.6631212326321,26.0290260283739));
#16329=CARTESIAN_POINT('Ctrl Pts',(1.58624560907291,-6.67254265715003,26.0290443535908));
#16330=CARTESIAN_POINT('Ctrl Pts',(1.58514848172257,-6.68181894203289,26.0291109728599));
#16331=CARTESIAN_POINT('Ctrl Pts',(1.58417352750872,-6.69006224490252,26.0291701735871));
#16332=CARTESIAN_POINT('Ctrl Pts',(1.58257090381714,-6.69829237126537,26.0292681713524));
#16333=CARTESIAN_POINT('Ctrl Pts',(1.58035806649011,-6.70635238271279,26.0294024407445));
#16334=CARTESIAN_POINT('Ctrl Pts',(1.57916454918057,-6.7106996354729,26.0294748603668));
#16335=CARTESIAN_POINT('Ctrl Pts',(1.57779442080559,-6.71499746492698,26.0295578317636));
#16336=CARTESIAN_POINT('Ctrl Pts',(1.57625656123137,-6.71922269938142,26.0296509586844));
#16337=CARTESIAN_POINT('',(1.41974152248314,-6.49569605876778,27.432));
#16338=CARTESIAN_POINT('Origin',(2.51551931327143,-6.88433565112087,27.4319999999994));
#16339=CARTESIAN_POINT('',(2.515519313271,-6.8843356511209,25.955721457172));
#16340=CARTESIAN_POINT('',(2.51551931327143,-6.88433565112087,27.4319999999994));
#16341=CARTESIAN_POINT('Origin',(-0.000420986725088723,-13.7968246230625,
-0.00421269407742564));
#16342=CARTESIAN_POINT('Origin',(1.51616036150637,-6.88433565112087,27.4319999999998));
#16343=CARTESIAN_POINT('',(1.51616036150594,-6.88433565112087,26.0332205371515));
#16344=CARTESIAN_POINT('',(1.51616036150637,-6.88433565112087,27.4319999999998));
#16345=CARTESIAN_POINT('Origin',(0.,-6.8843356511209,0.));
#16346=CARTESIAN_POINT('Origin',(1.57625656123139,-6.71922269938127,27.4319999999998));
#16347=CARTESIAN_POINT('Origin',(-0.00316823058453514,-11.0586552055069,
-0.0531056762106941));
#16348=CARTESIAN_POINT('Origin',(1.27456057433151,-6.66225588406201,27.432));
#16349=CARTESIAN_POINT('',(1.27456057433108,-6.49569605876776,26.0461668796032));
#16350=CARTESIAN_POINT('',(1.27456057433151,-6.49569605876778,27.432));
#16351=CARTESIAN_POINT('',(1.11804553558272,-6.60528906874258,26.0533546392426));
#16352=CARTESIAN_POINT('Ctrl Pts',(1.11804553558307,-6.60528906874271,26.0533546392426));
#16353=CARTESIAN_POINT('Ctrl Pts',(1.12103446249559,-6.59707705954213,26.0532263733652));
#16354=CARTESIAN_POINT('Ctrl Pts',(1.12469369229164,-6.58904702655386,26.0530682872682));
#16355=CARTESIAN_POINT('Ctrl Pts',(1.1289681221022,-6.58135462785479,26.0528830160049));
#16356=CARTESIAN_POINT('Ctrl Pts',(1.13324290149652,-6.57366160003377,26.0526977295893));
#16357=CARTESIAN_POINT('Ctrl Pts',(1.13813245925257,-6.56630722818087,26.0524852535604));
#16358=CARTESIAN_POINT('Ctrl Pts',(1.14353599672992,-6.55942235127054,26.0522482236182));
#16359=CARTESIAN_POINT('Ctrl Pts',(1.14425324207326,-6.55850847847442,26.0522167611507));
#16360=CARTESIAN_POINT('Ctrl Pts',(1.14497948490113,-6.55760283000169,26.05218486607));
#16361=CARTESIAN_POINT('Ctrl Pts',(1.14571443815834,-6.55670566570461,26.0521525445399));
#16362=CARTESIAN_POINT('Ctrl Pts',(1.15125497705314,-6.54994227819087,26.0519088845621));
#16363=CARTESIAN_POINT('Ctrl Pts',(1.1573681336888,-6.54357306166496,26.0516377375743));
#16364=CARTESIAN_POINT('Ctrl Pts',(1.16395025946269,-6.53772663590452,26.051343616843));
#16365=CARTESIAN_POINT('Ctrl Pts',(1.17053298993685,-6.53187967303261,26.0510494690908));
#16366=CARTESIAN_POINT('Ctrl Pts',(1.17758396244725,-6.5265563354955,26.0507323433737));
#16367=CARTESIAN_POINT('Ctrl Pts',(1.18496464466155,-6.52184667927605,26.0503967542022));
#16368=CARTESIAN_POINT('Ctrl Pts',(1.18593206127622,-6.52122936511135,26.0503527671383));
#16369=CARTESIAN_POINT('Ctrl Pts',(1.18690510423288,-6.52062253153143,26.0503084628642));
#16370=CARTESIAN_POINT('Ctrl Pts',(1.18788342971762,-6.52002632312747,26.0502638515464));
#16371=CARTESIAN_POINT('Ctrl Pts',(1.19584136977672,-6.51517661736448,26.0499009721171));
#16372=CARTESIAN_POINT('Ctrl Pts',(1.20426513104066,-6.51096499951925,26.0495126765159));
#16373=CARTESIAN_POINT('Ctrl Pts',(1.2129917086171,-6.5074933234193,26.0491063148917));
#16374=CARTESIAN_POINT('Ctrl Pts',(1.22171828619354,-6.50402164731935,26.0486999532675));
#16375=CARTESIAN_POINT('Ctrl Pts',(1.2307464285142,-6.50129044572284,26.0482755256203));
#16376=CARTESIAN_POINT('Ctrl Pts',(1.23988919517365,-6.49934464789538,26.047840382099));
#16377=CARTESIAN_POINT('Ctrl Pts',(1.24785857842602,-6.49764857391731,26.0474610849322));
#16378=CARTESIAN_POINT('Ctrl Pts',(1.25601438581795,-6.49652853241155,26.0470690549585));
#16379=CARTESIAN_POINT('Ctrl Pts',(1.26420465240645,-6.49601831224646,26.0466715531568));
#16380=CARTESIAN_POINT('Ctrl Pts',(1.26765453294,-6.49580339877614,26.0465041185912));
#16381=CARTESIAN_POINT('Ctrl Pts',(1.27111039084266,-6.49569605876778,26.0463357131928));
#16382=CARTESIAN_POINT('Ctrl Pts',(1.27456057433108,-6.49569605876777,26.0461668796032));
#16383=CARTESIAN_POINT('',(1.11804553558315,-6.60528906874258,27.432));
#16384=CARTESIAN_POINT('Origin',(1.27456057433151,-6.49569605876778,27.432));
#16385=CARTESIAN_POINT('Origin',(0.,-6.49569605876775,0.));
#16386=CARTESIAN_POINT('Origin',(1.03031472940818,-6.84632747769874,27.432));
#16387=CARTESIAN_POINT('Origin',(5.20520537479474E-5,-9.67695020546374,
0.00128786158793304));
#16388=CARTESIAN_POINT('Origin',(1.89451974084531,-7.53537652866758,27.4319999999997));
#16389=CARTESIAN_POINT('',(2.23363565813296,-7.65880462852638,25.9814969839017));
#16390=CARTESIAN_POINT('',(2.23363565813339,-7.65880462852638,27.432));
#16391=CARTESIAN_POINT('',(1.94474447683825,-7.17800896286548,26.0047165471492));
#16392=CARTESIAN_POINT('',(1.94474447683868,-7.17800896286548,27.4319999999997));
#16393=CARTESIAN_POINT('Ctrl Pts',(1.94474447683828,-7.17800896286542,26.0047165471494));
#16394=CARTESIAN_POINT('Ctrl Pts',(1.97445579346254,-7.18218461610387,26.0024946071871));
#16395=CARTESIAN_POINT('Ctrl Pts',(2.0043539541165,-7.19025063809253,26.0002055231238));
#16396=CARTESIAN_POINT('Ctrl Pts',(2.07717989960236,-7.22043523259437,25.994511502725));
#16397=CARTESIAN_POINT('Ctrl Pts',(2.11778923169758,-7.24824554657195,25.9912161699605));
#16398=CARTESIAN_POINT('Ctrl Pts',(2.18182192947338,-7.31235754563142,25.9859191780455));
#16399=CARTESIAN_POINT('Ctrl Pts',(2.20955505385306,-7.35289638626903,25.9835625173257));
#16400=CARTESIAN_POINT('Ctrl Pts',(2.24634429736412,-7.44175104057896,25.9804078475622));
#16401=CARTESIAN_POINT('Ctrl Pts',(2.25539936231613,-7.49006753666087,25.9796167695801));
#16402=CARTESIAN_POINT('Ctrl Pts',(2.25539936231613,-7.53537652866758,25.9796167695801));
#16403=CARTESIAN_POINT('Ctrl Pts',(2.25539936231613,-7.57575816120769,25.9796167695801));
#16404=CARTESIAN_POINT('Ctrl Pts',(2.24828582266216,-7.6185536322925,25.9802375056696));
#16405=CARTESIAN_POINT('Ctrl Pts',(2.23363565813338,-7.65880462852653,25.9814969839018));
#16406=CARTESIAN_POINT('Origin',(1.59597767698316,-8.35561410788657,27.4319999999998));
#16407=CARTESIAN_POINT('',(1.59597767698273,-8.71649372935708,26.0284492244993));
#16408=CARTESIAN_POINT('',(1.59597767698316,-8.71649372935708,27.4319999999998));
#16409=CARTESIAN_POINT('',(1.93509359427059,-8.47904220774527,26.0054364808433));
#16410=CARTESIAN_POINT('',(1.93509359427102,-8.47904220774527,27.4319999999997));
#16411=CARTESIAN_POINT('Ctrl Pts',(1.93509359427096,-8.4790422077454,26.0054364808436));
#16412=CARTESIAN_POINT('Ctrl Pts',(1.93330341915748,-8.48396067344652,26.0055696897747));
#16413=CARTESIAN_POINT('Ctrl Pts',(1.93140520253629,-8.48884284912114,26.0057107527781));
#16414=CARTESIAN_POINT('Ctrl Pts',(1.91100173043814,-8.5381161422481,26.007224507619));
#16415=CARTESIAN_POINT('Ctrl Pts',(1.88325785767842,-8.57866580739572,26.0092614621502));
#16416=CARTESIAN_POINT('Ctrl Pts',(1.81921304513536,-8.64276853406465,26.0138196108767));
#16417=CARTESIAN_POINT('Ctrl Pts',(1.77861272890292,-8.67056858397496,26.0166453909149));
#16418=CARTESIAN_POINT('Ctrl Pts',(1.68966168809246,-8.70743109202842,26.0225737392713));
#16419=CARTESIAN_POINT('Ctrl Pts',(1.641310588298,-8.71649372935709,26.0256695616058));
#16420=CARTESIAN_POINT('Ctrl Pts',(1.59597767698316,-8.71649372935709,26.0284492244996));
#16421=CARTESIAN_POINT('Origin',(-0.306199765510384,-7.77265471935663,27.432));
#16422=CARTESIAN_POINT('',(-0.306199765510815,-7.77265471935663,26.0755355742002));
#16423=CARTESIAN_POINT('',(-0.306199765510384,-7.77265471935663,27.432));
#16424=CARTESIAN_POINT('Origin',(4.80980058538416E-6,-6.93136435548834,
-0.00035220867896868));
#16425=CARTESIAN_POINT('Origin',(0.693159186254899,-7.77265471935663,27.432));
#16426=CARTESIAN_POINT('',(0.693159186254469,-7.77265471935663,26.0681193053948));
#16427=CARTESIAN_POINT('',(0.693159186254899,-7.77265471935663,27.432));
#16428=CARTESIAN_POINT('Origin',(0.,-7.77265471935663,0.));
#16429=CARTESIAN_POINT('Origin',(0.633062986529875,-7.9377676710961,27.432));
#16430=CARTESIAN_POINT('Origin',(0.00050811146186866,-9.67569638000616,
0.0186305338844139));
#16431=CARTESIAN_POINT('Origin',(-0.134339559012431,-8.71649372935708,27.432));
#16432=CARTESIAN_POINT('Origin',(0.,-8.71649372935708,0.));
#16433=CARTESIAN_POINT('Origin',(1.93509359427102,-8.47904220774527,27.4319999999997));
#16434=CARTESIAN_POINT('Origin',(0.0117441402215629,-13.7634009082281,-194.963090616663));
#16435=CARTESIAN_POINT('Origin',(1.94474447683868,-7.17800896286548,27.4319999999997));
#16436=CARTESIAN_POINT('Origin',(0.000105272415967667,-6.90470774651098,
-0.512300848302636));
#16437=CARTESIAN_POINT('Origin',(2.34365910677381,-5.9404966411204,27.432));
#16438=CARTESIAN_POINT('Origin',(0.,-5.94049664112042,0.));
#16439=CARTESIAN_POINT('Origin',(0.274225953490026,-6.17794816273243,27.432));
#16440=CARTESIAN_POINT('Origin',(2.31836480480096E-6,-6.93137081041626,
-196.838673546703));
#16441=CARTESIAN_POINT('Origin',(0.288891181294382,-7.41217344343619,27.432));
#16442=CARTESIAN_POINT('Origin',(8.19816643390925E-6,-7.37157358839081,
-0.514518939571));
#16443=CARTESIAN_POINT('Origin',(0.,-73.5076,0.));
#16444=CARTESIAN_POINT('Origin',(-3.8012386981594,-6.30137626259123,27.4319999999997));
#16445=CARTESIAN_POINT('',(-3.8012386981604,-5.94049664112043,25.7987964474583));
#16446=CARTESIAN_POINT('',(-3.8012386981594,-5.94049664112042,27.4319999999997));
#16447=CARTESIAN_POINT('',(-4.14035461544859,-6.17794816273246,25.7465488451583));
#16448=CARTESIAN_POINT('',(-4.14035461544748,-6.17794816273246,27.432));
#16449=CARTESIAN_POINT('Ctrl Pts',(-4.14035461544765,-6.1779481627328,25.7465488451583));
#16450=CARTESIAN_POINT('Ctrl Pts',(-4.13853613021595,-6.17295191562108,
25.7468412794479));
#16451=CARTESIAN_POINT('Ctrl Pts',(-4.13660636125172,-6.16799367762682,
25.747151412347));
#16452=CARTESIAN_POINT('Ctrl Pts',(-4.11612473857417,-6.1186271231225,25.7504403817435));
#16453=CARTESIAN_POINT('Ctrl Pts',(-4.08834737176778,-6.07812408113152,
25.7548786492327));
#16454=CARTESIAN_POINT('Ctrl Pts',(-4.02428517439673,-6.01406188376048,
25.7649665400282));
#16455=CARTESIAN_POINT('Ctrl Pts',(-3.98365303782638,-5.98629953163405,
25.7712988498757));
#16456=CARTESIAN_POINT('Ctrl Pts',(-3.89474826397818,-5.94951791188519,
25.7848845623868));
#16457=CARTESIAN_POINT('Ctrl Pts',(-3.84647542051267,-5.94049664112043,
25.7921311915836));
#16458=CARTESIAN_POINT('Ctrl Pts',(-3.8012386981594,-5.94049664112043,25.7987964474585));
#16459=CARTESIAN_POINT('Origin',(-2.07092146216392,-6.30137626259123,27.4319999999996));
#16460=CARTESIAN_POINT('',(-1.73180554487627,-6.42480436245001,26.0197648592856));
#16461=CARTESIAN_POINT('',(-1.73180554487584,-6.42480436245001,27.4319999999999));
#16462=CARTESIAN_POINT('',(-2.07092146216446,-5.94049664112041,25.994972553848));
#16463=CARTESIAN_POINT('',(-2.07092146216392,-5.9404966411204,27.4319999999996));
#16464=CARTESIAN_POINT('Ctrl Pts',(-2.07092146216392,-5.94049664112042,
25.9949725538484));
#16465=CARTESIAN_POINT('Ctrl Pts',(-2.02565079587898,-5.94049664112035,
25.9985790971606));
#16466=CARTESIAN_POINT('Ctrl Pts',(-1.97733911111438,-5.94953559083106,
26.0022966555945));
#16467=CARTESIAN_POINT('Ctrl Pts',(-1.88842052724259,-5.98634781377435,
26.0089055755554));
#16468=CARTESIAN_POINT('Ctrl Pts',(-1.84781461144272,-6.01412225824434,
26.0118036411467));
#16469=CARTESIAN_POINT('Ctrl Pts',(-1.78372330332947,-6.07821356635759,
26.0162771180725));
#16470=CARTESIAN_POINT('Ctrl Pts',(-1.7559481642718,-6.11877929027088,26.0181532905424));
#16471=CARTESIAN_POINT('Ctrl Pts',(-1.71910716522096,-6.2076931086887,26.0206134662523));
#16472=CARTESIAN_POINT('Ctrl Pts',(-1.7100418406931,-6.25604123728692,26.0212042511652));
#16473=CARTESIAN_POINT('Ctrl Pts',(-1.7100418406931,-6.30137626259124,26.0212042511652));
#16474=CARTESIAN_POINT('Ctrl Pts',(-1.71004184069311,-6.34175145456393,
26.0212042511652));
#16475=CARTESIAN_POINT('Ctrl Pts',(-1.71715359966824,-6.38454847384126,
26.0207400533388));
#16476=CARTESIAN_POINT('Ctrl Pts',(-1.73180554487585,-6.42480436245017,
26.0197648592857));
#16477=CARTESIAN_POINT('Origin',(-2.81860289195435,-8.35561410788657,27.432));
#16478=CARTESIAN_POINT('',(-2.81860289195478,-8.71649372935708,25.9245596204689));
#16479=CARTESIAN_POINT('',(-2.81860289195435,-8.71649372935708,27.432));
#16480=CARTESIAN_POINT('',(-2.47948697466692,-8.47904220774524,25.9591883178234));
#16481=CARTESIAN_POINT('',(-2.47948697466649,-8.47904220774524,27.4319999999996));
#16482=CARTESIAN_POINT('Ctrl Pts',(-2.47948697466655,-8.47904220774539,
25.9591883178238));
#16483=CARTESIAN_POINT('Ctrl Pts',(-2.48127016634398,-8.48394148661369,
25.9590179966072));
#16484=CARTESIAN_POINT('Ctrl Pts',(-2.48316051044314,-8.4888046275687,25.9588372557841));
#16485=CARTESIAN_POINT('Ctrl Pts',(-2.50353617632185,-8.53803458580152,
25.9568865881412));
#16486=CARTESIAN_POINT('Ctrl Pts',(-2.53124614061308,-8.57855371372092,
25.954212289626));
#16487=CARTESIAN_POINT('Ctrl Pts',(-2.59527693429706,-8.64271337170564,
25.9478880176867));
#16488=CARTESIAN_POINT('Ctrl Pts',(-2.63593395404322,-8.67055411005893,
25.9438078924707));
#16489=CARTESIAN_POINT('Ctrl Pts',(-2.72494725337074,-8.70744328106339,
25.9346096604108));
#16490=CARTESIAN_POINT('Ctrl Pts',(-2.77330200793706,-8.71649372935709,
25.9294848807074));
#16491=CARTESIAN_POINT('Ctrl Pts',(-2.81860289195435,-8.71649372935709,
25.9245596204689));
#16492=CARTESIAN_POINT('Origin',(-4.14035461544748,-6.17794816273246,27.432));
#16493=CARTESIAN_POINT('Origin',(-0.119276906042105,4.86987221912099,-188.054460439309));
#16494=CARTESIAN_POINT('Origin',(-4.54892012795016,-8.71649372935708,27.432));
#16495=CARTESIAN_POINT('Origin',(0.,-8.71649372935708,0.));
#16496=CARTESIAN_POINT('Origin',(-2.47948697466649,-8.47904220774524,27.4319999999996));
#16497=CARTESIAN_POINT('Origin',(-0.0120303754226056,-1.69976083906543,
-194.915632611861));
#16498=CARTESIAN_POINT('Origin',(-2.07092146216392,-5.94049664112042,27.4319999999996));
#16499=CARTESIAN_POINT('Origin',(0.,-5.9404966411204,0.));
#16500=CARTESIAN_POINT('Origin',(0.,-73.5076,0.));
#16501=CARTESIAN_POINT('',(-3.47982159550796,-8.16129431171214,25.8441125876128));
#16502=CARTESIAN_POINT('Origin',(0.,-8.16129431171214,0.));
#16503=CARTESIAN_POINT('',(-3.29653503335457,-6.60528906874482,25.8681304030971));
#16504=CARTESIAN_POINT('Origin',(-0.0574956826298151,2.29389872667189,-191.430235841408));
#16505=CARTESIAN_POINT('',(-3.14001999460632,-6.49569605877014,25.8875952574057));
#16506=CARTESIAN_POINT('Ctrl Pts',(-3.29653503335502,-6.60528906874466,
25.8681304030971));
#16507=CARTESIAN_POINT('Ctrl Pts',(-3.29355163274793,-6.5970922429435,25.8685105961945));
#16508=CARTESIAN_POINT('Ctrl Pts',(-3.28990147519521,-6.58907971254542,
25.8689769976669));
#16509=CARTESIAN_POINT('Ctrl Pts',(-3.28564105767213,-6.58140613827777,
25.8695182287522));
#16510=CARTESIAN_POINT('Ctrl Pts',(-3.28137930905549,-6.57373016653493,
25.8700596289357));
#16511=CARTESIAN_POINT('Ctrl Pts',(-3.27650745242721,-6.56639432354615,
25.8706759054979));
#16512=CARTESIAN_POINT('Ctrl Pts',(-3.2711274779456,-6.5595280727638,25.8713556690078));
#16513=CARTESIAN_POINT('Ctrl Pts',(-3.27039974797208,-6.55859929949228,
25.871447618195));
#16514=CARTESIAN_POINT('Ctrl Pts',(-3.2696627809311,-6.55767906826433,25.8715407290035));
#16515=CARTESIAN_POINT('Ctrl Pts',(-3.26891688314673,-6.55676764999646,
25.8716349732447));
#16516=CARTESIAN_POINT('Ctrl Pts',(-3.26336740858408,-6.54998670413574,
25.8723361497736));
#16517=CARTESIAN_POINT('Ctrl Pts',(-3.25724578705905,-6.5436052552422,25.873109003126));
#16518=CARTESIAN_POINT('Ctrl Pts',(-3.25065739506098,-6.53775069934186,
25.8739367848223));
#16519=CARTESIAN_POINT('Ctrl Pts',(-3.24406682081912,-6.53189420426301,
25.874764840701));
#16520=CARTESIAN_POINT('Ctrl Pts',(-3.23700999050808,-6.52656567852879,
25.875647861317));
#16521=CARTESIAN_POINT('Ctrl Pts',(-3.2296267624176,-6.52185359574774,25.8765690815424));
#16522=CARTESIAN_POINT('Ctrl Pts',(-3.22873901445968,-6.52128702218192,
25.8766798476414));
#16523=CARTESIAN_POINT('Ctrl Pts',(-3.22784657922314,-6.52072930737335,
25.8767911660032));
#16524=CARTESIAN_POINT('Ctrl Pts',(-3.22694972365762,-6.5201805603477,25.8769030074844));
#16525=CARTESIAN_POINT('Ctrl Pts',(-3.21899904308127,-6.51531588370863,
25.8778944891977));
#16526=CARTESIAN_POINT('Ctrl Pts',(-3.21058572140309,-6.51109127760728,
25.8789405230786));
#16527=CARTESIAN_POINT('Ctrl Pts',(-3.20187148631304,-6.50760605905393,
25.8800186216765));
#16528=CARTESIAN_POINT('Ctrl Pts',(-3.19315725122299,-6.50412084050059,
25.8810967202744));
#16529=CARTESIAN_POINT('Ctrl Pts',(-3.18414331911176,-6.5013755160139,25.8822068835893));
#16530=CARTESIAN_POINT('Ctrl Pts',(-3.17501443033165,-6.49941373696988,
25.8833266241705));
#16531=CARTESIAN_POINT('Ctrl Pts',(-3.16698548919387,-6.49768833436621,
25.8843114462483));
#16532=CARTESIAN_POINT('Ctrl Pts',(-3.1587682304718,-6.49654813372328,25.8853156351911));
#16533=CARTESIAN_POINT('Ctrl Pts',(-3.1505154759895,-6.49602706504496,25.886320048665));
#16534=CARTESIAN_POINT('Ctrl Pts',(-3.14701924036618,-6.4958063170657,25.8867455631008));
#16535=CARTESIAN_POINT('Ctrl Pts',(-3.14351677283593,-6.49569605877014,
25.8871711178343));
#16536=CARTESIAN_POINT('Ctrl Pts',(-3.14001999460632,-6.49569605877015,
25.8875952574057));
#16537=CARTESIAN_POINT('',(-2.99483904645491,-6.49569605877014,25.9047920830029));
#16538=CARTESIAN_POINT('Origin',(0.,-6.49569605877014,0.));
#16539=CARTESIAN_POINT('',(-2.83832400770644,-6.71922269938391,25.9224078859403));
#16540=CARTESIAN_POINT('Ctrl Pts',(-2.99483904645491,-6.49569605877015,
25.904792083003));
#16541=CARTESIAN_POINT('Ctrl Pts',(-2.98604988693302,-6.49569605877018,
25.9058081929967));
#16542=CARTESIAN_POINT('Ctrl Pts',(-2.97720115569464,-6.49639608767757,
25.9068261670284));
#16543=CARTESIAN_POINT('Ctrl Pts',(-2.96845899341274,-6.49779838741705,
25.9078277470632));
#16544=CARTESIAN_POINT('Ctrl Pts',(-2.95971734185864,-6.49920060523247,
25.9088292685845));
#16545=CARTESIAN_POINT('Ctrl Pts',(-2.95108333421324,-6.50130485849879,
25.9098143980243));
#16546=CARTESIAN_POINT('Ctrl Pts',(-2.94271565014682,-6.50406193045269,
25.9107648805478));
#16547=CARTESIAN_POINT('Ctrl Pts',(-2.94162256813388,-6.5044220905325,25.9108890433796));
#16548=CARTESIAN_POINT('Ctrl Pts',(-2.94053400712044,-6.50479332166405,
25.9110126149773));
#16549=CARTESIAN_POINT('Ctrl Pts',(-2.93945029664687,-6.50517545308494,
25.9111355546478));
#16550=CARTESIAN_POINT('Ctrl Pts',(-2.93118716642089,-6.50808914799823,
25.9120729512419));
#16551=CARTESIAN_POINT('Ctrl Pts',(-2.92309662982777,-6.5116796685772,25.912985794272));
#16552=CARTESIAN_POINT('Ctrl Pts',(-2.91533613546422,-6.51589515659296,
25.9138587429305));
#16553=CARTESIAN_POINT('Ctrl Pts',(-2.90757697996784,-6.52010991733822,
25.914731540985));
#16554=CARTESIAN_POINT('Ctrl Pts',(-2.90014873115125,-6.52494893117182,
25.9155644584321));
#16555=CARTESIAN_POINT('Ctrl Pts',(-2.89318495645261,-6.53031414924276,
25.9163421624029));
#16556=CARTESIAN_POINT('Ctrl Pts',(-2.89221146664238,-6.53106417137123,
25.9164508802928));
#16557=CARTESIAN_POINT('Ctrl Pts',(-2.89124700240809,-6.53182441096177,
25.91655851919));
#16558=CARTESIAN_POINT('Ctrl Pts',(-2.8902918757435,-6.53259453863649,25.9166650372072));
#16559=CARTESIAN_POINT('Ctrl Pts',(-2.88349863179219,-6.53807199556647,
25.9174226360709));
#16560=CARTESIAN_POINT('Ctrl Pts',(-2.87708906319131,-6.54412661882051,
25.9181334301957));
#16561=CARTESIAN_POINT('Ctrl Pts',(-2.87119418361552,-6.55065784064362,
25.9187863014831));
#16562=CARTESIAN_POINT('Ctrl Pts',(-2.86530048605939,-6.55718775285004,
25.9194390418591));
#16563=CARTESIAN_POINT('Ctrl Pts',(-2.85992202958957,-6.56419327834773,
25.9200338826243));
#16564=CARTESIAN_POINT('Ctrl Pts',(-2.85515199602751,-6.57153817165499,
25.920559712367));
#16565=CARTESIAN_POINT('Ctrl Pts',(-2.85445801481418,-6.57260676329126,
25.920636214127));
#16566=CARTESIAN_POINT('Ctrl Pts',(-2.85377683606089,-6.57368248947024,
25.9207112551534));
#16567=CARTESIAN_POINT('Ctrl Pts',(-2.85310866708237,-6.57476488472837,
25.9207848012288));
#16568=CARTESIAN_POINT('Ctrl Pts',(-2.84853944267849,-6.58216676507169,
25.9212877406543));
#16569=CARTESIAN_POINT('Ctrl Pts',(-2.84452073762891,-6.58998235174926,
25.9217273547419));
#16570=CARTESIAN_POINT('Ctrl Pts',(-2.84114196992495,-6.59807345603279,
25.922097525811));
#16571=CARTESIAN_POINT('Ctrl Pts',(-2.83776363548719,-6.60616352277769,
25.9224676494123));
#16572=CARTESIAN_POINT('Ctrl Pts',(-2.8350255217226,-6.61452803348443,25.9227683478036));
#16573=CARTESIAN_POINT('Ctrl Pts',(-2.83296944329677,-6.62300786532066,
25.9229935056573));
#16574=CARTESIAN_POINT('Ctrl Pts',(-2.83267407255108,-6.62422605535723,
25.9230258512344));
#16575=CARTESIAN_POINT('Ctrl Pts',(-2.83239269161826,-6.62544660538507,
25.9230566378489));
#16576=CARTESIAN_POINT('Ctrl Pts',(-2.83212533756036,-6.62666902778762,
25.9230858473707));
#16577=CARTESIAN_POINT('Ctrl Pts',(-2.83014108332478,-6.63574162929957,
25.9233026352427));
#16578=CARTESIAN_POINT('Ctrl Pts',(-2.82890600766917,-6.64504884472927,
25.9234355837559));
#16579=CARTESIAN_POINT('Ctrl Pts',(-2.82846448404262,-6.65440219805072,
25.9234836656352));
#16580=CARTESIAN_POINT('Ctrl Pts',(-2.82802296041607,-6.66375555137217,
25.9235317475145));
#16581=CARTESIAN_POINT('Ctrl Pts',(-2.82837509095446,-6.67315364782026,
25.92349496276));
#16582=CARTESIAN_POINT('Ctrl Pts',(-2.82950229820537,-6.6824037147207,25.9233722840967));
#16583=CARTESIAN_POINT('Ctrl Pts',(-2.83050058783001,-6.69059586022591,
25.923263636076));
#16584=CARTESIAN_POINT('Ctrl Pts',(-2.83211933265879,-6.69877298983038,
25.9230862244867));
#16585=CARTESIAN_POINT('Ctrl Pts',(-2.83434024192632,-6.7067790145337,25.9228435144729));
#16586=CARTESIAN_POINT('Ctrl Pts',(-2.83550590448341,-6.71098104266887,
25.9227161261192));
#16587=CARTESIAN_POINT('Ctrl Pts',(-2.83683657416436,-6.71513600931251,
25.9225707496046));
#16588=CARTESIAN_POINT('Ctrl Pts',(-2.83832400770695,-6.71922269938372,
25.9224078859403));
#16589=CARTESIAN_POINT('',(-3.32330655675982,-8.05170130173748,25.8647046630648));
#16590=CARTESIAN_POINT('Origin',(-0.03791555774525,0.974836476930119,-192.736729294503));
#16591=CARTESIAN_POINT('Ctrl Pts',(-3.32330655676036,-8.05170130173729,
25.8647046630648));
#16592=CARTESIAN_POINT('Ctrl Pts',(-3.32628772155065,-8.05989198468231,
25.8643216188885));
#16593=CARTESIAN_POINT('Ctrl Pts',(-3.32993463283106,-8.06789859750961,
25.8638508107442));
#16594=CARTESIAN_POINT('Ctrl Pts',(-3.33419076046539,-8.07556662907552,
25.8633019966676));
#16595=CARTESIAN_POINT('Ctrl Pts',(-3.33844829513998,-8.08323719562866,
25.8627530011578));
#16596=CARTESIAN_POINT('Ctrl Pts',(-3.34331491504015,-8.09056799656464,
25.8621259481309));
#16597=CARTESIAN_POINT('Ctrl Pts',(-3.34868860752307,-8.0974297388106,25.8614306053038));
#16598=CARTESIAN_POINT('Ctrl Pts',(-3.34941960065303,-8.09836315404739,
25.8613360165585));
#16599=CARTESIAN_POINT('Ctrl Pts',(-3.35015991637763,-8.099287940198,25.861240164134));
#16600=CARTESIAN_POINT('Ctrl Pts',(-3.35090924308524,-8.10020382222073,
25.8611430726179));
#16601=CARTESIAN_POINT('Ctrl Pts',(-3.35645275599859,-8.1069795100063,25.8604247903685));
#16602=CARTESIAN_POINT('Ctrl Pts',(-3.36256709225747,-8.11335604909613,
25.8596293390504));
#16603=CARTESIAN_POINT('Ctrl Pts',(-3.36914674644083,-8.11920638359092,
25.8587719962737));
#16604=CARTESIAN_POINT('Ctrl Pts',(-3.37572891987411,-8.12505895809016,
25.8579143252334));
#16605=CARTESIAN_POINT('Ctrl Pts',(-3.38277594224888,-8.13038419952754,
25.856994715331));
#16606=CARTESIAN_POINT('Ctrl Pts',(-3.39014788753786,-8.13509403009346,
25.8560284617318));
#16607=CARTESIAN_POINT('Ctrl Pts',(-3.39103950586256,-8.13566367230785,
25.8559115957783));
#16608=CARTESIAN_POINT('Ctrl Pts',(-3.39193584545124,-8.13622436613148,
25.855794047507));
#16609=CARTESIAN_POINT('Ctrl Pts',(-3.39283663456694,-8.13677600137747,
25.8556758439789));
#16610=CARTESIAN_POINT('Ctrl Pts',(-3.40077919405817,-8.14163995419661,
25.8546336038611));
#16611=CARTESIAN_POINT('Ctrl Pts',(-3.40918258080237,-8.14586420520276,
25.8535261193517));
#16612=CARTESIAN_POINT('Ctrl Pts',(-3.41788511420254,-8.14935029313074,
25.8523755838862));
#16613=CARTESIAN_POINT('Ctrl Pts',(-3.4265876476027,-8.15283638105871,25.8512250484207));
#16614=CARTESIAN_POINT('Ctrl Pts',(-3.43558811299829,-8.15558380712578,
25.8500314619991));
#16615=CARTESIAN_POINT('Ctrl Pts',(-3.444702101002,-8.15754970839559,25.8488170180567));
#16616=CARTESIAN_POINT('Ctrl Pts',(-3.45274752739098,-8.15928511927695,
25.8477449605404));
#16617=CARTESIAN_POINT('Ctrl Pts',(-3.46098082739164,-8.16043251884309,
25.8466437182488));
#16618=CARTESIAN_POINT('Ctrl Pts',(-3.46924887002126,-8.16095841032121,
25.845533929296));
#16619=CARTESIAN_POINT('Ctrl Pts',(-3.47277099149017,-8.16118243597618,
25.8450611678853));
#16620=CARTESIAN_POINT('Ctrl Pts',(-3.47629927897631,-8.16129431171212,
25.8445868555178));
#16621=CARTESIAN_POINT('Ctrl Pts',(-3.47982159550796,-8.16129431171213,
25.8441125876128));
#16622=CARTESIAN_POINT('Origin',(-3.62500254366004,-8.16129431171214,53.8479999999997));
#16623=CARTESIAN_POINT('',(-3.47982159550753,-8.16129431171214,26.6981762984558));
#16624=CARTESIAN_POINT('',(-3.47982159550862,-8.16129431171214,53.8479999999997));
#16625=CARTESIAN_POINT('Origin',(0.,-8.16129431171214,0.));
#16626=CARTESIAN_POINT('Origin',(-3.29653503335513,-6.60528906874482,53.8479999999997));
#16627=CARTESIAN_POINT('',(-3.29653503335414,-6.60528906874482,26.72142647341));
#16628=CARTESIAN_POINT('Origin',(-0.0539360021858648,2.30367859284946,-197.990307955962));
#16629=CARTESIAN_POINT('',(-3.29653503335513,-6.60528906874482,53.8479999999997));
#16630=CARTESIAN_POINT('Origin',(-3.14001999460688,-6.6622558840642,53.8479999999999));
#16631=CARTESIAN_POINT('',(-3.14001999460589,-6.49569605877014,26.7402702012054));
#16632=CARTESIAN_POINT('Ctrl Pts',(-3.14001999460589,-6.49569605877015,
26.7402702012054));
#16633=CARTESIAN_POINT('Ctrl Pts',(-3.1488191702827,-6.4956960587701,26.7392369435998));
#16634=CARTESIAN_POINT('Ctrl Pts',(-3.15767689543388,-6.49639767484394,
26.7381924155668));
#16635=CARTESIAN_POINT('Ctrl Pts',(-3.1664268801426,-6.49780269376894,26.7371562240251));
#16636=CARTESIAN_POINT('Ctrl Pts',(-3.17517678121555,-6.49920769926423,
26.7361200423878));
#16637=CARTESIAN_POINT('Ctrl Pts',(-3.1838178569037,-6.50131593774875,26.7350921970825));
#16638=CARTESIAN_POINT('Ctrl Pts',(-3.19219138868498,-6.50407775333201,
26.7340922944658));
#16639=CARTESIAN_POINT('Ctrl Pts',(-3.19328394140197,-6.50443810654952,
26.7339618302424));
#16640=CARTESIAN_POINT('Ctrl Pts',(-3.19437196320816,-6.50480951762784,
26.7338318417218));
#16641=CARTESIAN_POINT('Ctrl Pts',(-3.19545512579727,-6.50519181550653,
26.7337023724549));
#16642=CARTESIAN_POINT('Ctrl Pts',(-3.20372978442124,-6.50811232298216,
26.7327133113512));
#16643=CARTESIAN_POINT('Ctrl Pts',(-3.21183053458493,-6.51171141222322,
26.7317418058702));
#16644=CARTESIAN_POINT('Ctrl Pts',(-3.21959977929409,-6.51593694041328,
26.7308061448951));
#16645=CARTESIAN_POINT('Ctrl Pts',(-3.22736775298049,-6.5201617773209,26.7298706369911));
#16646=CARTESIAN_POINT('Ctrl Pts',(-3.23480335196702,-6.52501234838073,
26.728970961866));
#16647=CARTESIAN_POINT('Ctrl Pts',(-3.24177290544418,-6.53039034444857,
26.7281253994286));
#16648=CARTESIAN_POINT('Ctrl Pts',(-3.2427344694278,-6.5311323270361,26.7280087402498));
#16649=CARTESIAN_POINT('Ctrl Pts',(-3.24368721240133,-6.53188428501759,
26.7278931110907));
#16650=CARTESIAN_POINT('Ctrl Pts',(-3.24463083414372,-6.53264590121804,
26.7277785599572));
#16651=CARTESIAN_POINT('Ctrl Pts',(-3.25192202187037,-6.53853076635387,
26.7268934448938));
#16652=CARTESIAN_POINT('Ctrl Pts',(-3.2587707092415,-6.54508132928967,26.7260605188436));
#16653=CARTESIAN_POINT('Ctrl Pts',(-3.26502066044175,-6.55217859783846,
26.7252970945294));
#16654=CARTESIAN_POINT('Ctrl Pts',(-3.27127061164199,-6.55927586638725,
26.7245336702151));
#16655=CARTESIAN_POINT('Ctrl Pts',(-3.27692084770924,-6.56691882582606,
26.7238397476368));
#16656=CARTESIAN_POINT('Ctrl Pts',(-3.2818612437607,-6.57494474250444,26.7232326395169));
#16657=CARTESIAN_POINT('Ctrl Pts',(-3.28607064325319,-6.58178311927442,
26.7227153610264));
#16658=CARTESIAN_POINT('Ctrl Pts',(-3.28981753641634,-6.58898622132904,
26.722254792006));
#16659=CARTESIAN_POINT('Ctrl Pts',(-3.2930180561961,-6.59642451956425,26.7218602614005));
#16660=CARTESIAN_POINT('Ctrl Pts',(-3.2942752393729,-6.59934632728575,26.7217052874357));
#16661=CARTESIAN_POINT('Ctrl Pts',(-3.29544860141099,-6.60230412151067,
26.7215605029674));
#16662=CARTESIAN_POINT('Ctrl Pts',(-3.29653503335497,-6.60528906874452,
26.72142647341));
#16663=CARTESIAN_POINT('',(-3.14001999460688,-6.49569605877014,53.8479999999999));
#16664=CARTESIAN_POINT('Origin',(-2.99483904645546,-6.49569605877014,53.8479999999999));
#16665=CARTESIAN_POINT('',(-2.99483904645448,-6.49569605877014,26.7569190133287));
#16666=CARTESIAN_POINT('Origin',(0.,-6.49569605877014,0.));
#16667=CARTESIAN_POINT('',(-2.99483904645546,-6.49569605877014,53.8479999999999));
#16668=CARTESIAN_POINT('Origin',(-2.99483904645546,-6.66225588406445,53.8479999999999));
#16669=CARTESIAN_POINT('',(-2.83832400770601,-6.71922269938391,26.7739741694669));
#16670=CARTESIAN_POINT('Ctrl Pts',(-2.8383240077069,-6.71922269938358,26.7739741694669));
#16671=CARTESIAN_POINT('Ctrl Pts',(-2.83535031273295,-6.71105253959025,
26.7742894125377));
#16672=CARTESIAN_POINT('Ctrl Pts',(-2.83299957248698,-6.70259076370276,
26.7745366280647));
#16673=CARTESIAN_POINT('Ctrl Pts',(-2.83133045381799,-6.6939909677382,26.7747129991209));
#16674=CARTESIAN_POINT('Ctrl Pts',(-2.82966138939106,-6.68539145124489,
26.7748893644455));
#16675=CARTESIAN_POINT('Ctrl Pts',(-2.82867413047415,-6.67665499801196,
26.7749948899037));
#16676=CARTESIAN_POINT('Ctrl Pts',(-2.82837643798522,-6.66794582108957,
26.7750267588431));
#16677=CARTESIAN_POINT('Ctrl Pts',(-2.82833717499765,-6.66679715823131,
26.7750309620724));
#16678=CARTESIAN_POINT('Ctrl Pts',(-2.8283098328581,-6.66564897123872,26.7750338840273));
#16679=CARTESIAN_POINT('Ctrl Pts',(-2.82829436174616,-6.66450163497332,
26.7750355182457));
#16680=CARTESIAN_POINT('Ctrl Pts',(-2.8281770570531,-6.65580232952357,26.7750479091774));
#16681=CARTESIAN_POINT('Ctrl Pts',(-2.82874490389417,-6.64703529469191,
26.7749864308833));
#16682=CARTESIAN_POINT('Ctrl Pts',(-2.83000156362019,-6.63836488880268,
26.7748534820682));
#16683=CARTESIAN_POINT('Ctrl Pts',(-2.83125836446463,-6.62969350925764,
26.7747205183233));
#16684=CARTESIAN_POINT('Ctrl Pts',(-2.83320398633801,-6.62111986910625,
26.7745160680046));
#16685=CARTESIAN_POINT('Ctrl Pts',(-2.8357905648614,-6.61280129980081,26.7742425306248));
#16686=CARTESIAN_POINT('Ctrl Pts',(-2.83613148392516,-6.61170488659171,
26.7742064775506));
#16687=CARTESIAN_POINT('Ctrl Pts',(-2.83648346733054,-6.6106128808583,26.7741692242921));
#16688=CARTESIAN_POINT('Ctrl Pts',(-2.83684634255612,-6.60952561840382,
26.7741307763433));
#16689=CARTESIAN_POINT('Ctrl Pts',(-2.83960635761554,-6.60125594184184,
26.7738383427186));
#16690=CARTESIAN_POINT('Ctrl Pts',(-2.84303748572811,-6.59315125675376,
26.7734729756253));
#16691=CARTESIAN_POINT('Ctrl Pts',(-2.84708790623562,-6.5853678097889,26.7730421470615));
#16692=CARTESIAN_POINT('Ctrl Pts',(-2.85113926529111,-6.5775825592734,26.7726112186678));
#16693=CARTESIAN_POINT('Ctrl Pts',(-2.85580969960795,-6.57011967198458,
26.772114798463));
#16694=CARTESIAN_POINT('Ctrl Pts',(-2.86100118274833,-6.5631115365686,26.7715603636404));
#16695=CARTESIAN_POINT('Ctrl Pts',(-2.86165469982663,-6.56222933468957,
26.7714905699773));
#16696=CARTESIAN_POINT('Ctrl Pts',(-2.86231642033745,-6.56135429707077,
26.7714198569905));
#16697=CARTESIAN_POINT('Ctrl Pts',(-2.8629861044557,-6.56048664957743,26.7713482395955));
#16698=CARTESIAN_POINT('Ctrl Pts',(-2.86833197674404,-6.55356049952506,
26.770776541034));
#16699=CARTESIAN_POINT('Ctrl Pts',(-2.87426017937969,-6.54701527171286,
26.7701397631968));
#16700=CARTESIAN_POINT('Ctrl Pts',(-2.88066950157966,-6.5409814414769,26.7694499860509));
#16701=CARTESIAN_POINT('Ctrl Pts',(-2.88708065886669,-6.534945883663,26.7687600114113));
#16702=CARTESIAN_POINT('Ctrl Pts',(-2.8939724108391,-6.52942276902587,26.7680170071095));
#16703=CARTESIAN_POINT('Ctrl Pts',(-2.90120788571586,-6.52450472747903,
26.7672330634915));
#16704=CARTESIAN_POINT('Ctrl Pts',(-2.90208655444725,-6.52390748550106,
26.7671378621735));
#16705=CARTESIAN_POINT('Ctrl Pts',(-2.9029702583552,-6.52331911343307,26.767042057106));
#16706=CARTESIAN_POINT('Ctrl Pts',(-2.90385872631525,-6.52273973177644,
26.7669456699416));
#16707=CARTESIAN_POINT('Ctrl Pts',(-2.91165923363107,-6.51765291823399,
26.7660994168241));
#16708=CARTESIAN_POINT('Ctrl Pts',(-2.91994032365346,-6.51319122296968,
26.7651966304368));
#16709=CARTESIAN_POINT('Ctrl Pts',(-2.92854192177034,-6.50945906910893,
26.7642554502871));
#16710=CARTESIAN_POINT('Ctrl Pts',(-2.93714351988722,-6.50572691524818,
26.7633142701374));
#16711=CARTESIAN_POINT('Ctrl Pts',(-2.9460643961385,-6.50272485098206,26.7623346962255));
#16712=CARTESIAN_POINT('Ctrl Pts',(-2.95511964132775,-6.50050130373249,
26.7613348680589));
#16713=CARTESIAN_POINT('Ctrl Pts',(-2.96330012922314,-6.49849255620774,
26.7604316255688));
#16714=CARTESIAN_POINT('Ctrl Pts',(-2.97169026860371,-6.49709480339873,
26.7595010975517));
#16715=CARTESIAN_POINT('Ctrl Pts',(-2.98013496720119,-6.49634637422445,
26.7585606368878));
#16716=CARTESIAN_POINT('Ctrl Pts',(-2.98502867881265,-6.49591265874031,
26.7580156389558));
#16717=CARTESIAN_POINT('Ctrl Pts',(-2.98994041682273,-6.49569605877018,
26.757467305428));
#16718=CARTESIAN_POINT('Ctrl Pts',(-2.99483904645448,-6.49569605877015,
26.7569190133287));
#16719=CARTESIAN_POINT('',(-2.83832400770699,-6.71922269938391,53.8479999999993));
#16720=CARTESIAN_POINT('Origin',(-3.32330655676037,-8.05170130173748,53.8479999999997));
#16721=CARTESIAN_POINT('',(-3.32330655675939,-8.05170130173748,26.7181101414338));
#16722=CARTESIAN_POINT('Origin',(-0.0355681310817269,0.981285811977752,
-199.256353335251));
#16723=CARTESIAN_POINT('',(-3.32330655676037,-8.05170130173748,53.8479999999997));
#16724=CARTESIAN_POINT('Origin',(-3.47982159550862,-7.9947344864181,53.8479999999997));
#16725=CARTESIAN_POINT('Ctrl Pts',(-3.47982159550753,-8.16129431171213,
26.6981762984558));
#16726=CARTESIAN_POINT('Ctrl Pts',(-3.47101905797183,-8.16129431171207,
26.6993236150316));
#16727=CARTESIAN_POINT('Ctrl Pts',(-3.46215680434601,-8.16059216358522,
26.7004737750014));
#16728=CARTESIAN_POINT('Ctrl Pts',(-3.45340124290307,-8.15918551368816,
26.7016060748986));
#16729=CARTESIAN_POINT('Ctrl Pts',(-3.4446464045589,-8.1577789799626,26.7027382812822));
#16730=CARTESIAN_POINT('Ctrl Pts',(-3.43599932822443,-8.15566821300049,
26.7038526305433));
#16731=CARTESIAN_POINT('Ctrl Pts',(-3.4276189995069,-8.15290232250578,26.7049284243444));
#16732=CARTESIAN_POINT('Ctrl Pts',(-3.42652792271427,-8.1525422174274,26.7050684873049));
#16733=CARTESIAN_POINT('Ctrl Pts',(-3.42544134401775,-8.15217107610206,
26.705207896722));
#16734=CARTESIAN_POINT('Ctrl Pts',(-3.42435959041194,-8.15178906735299,
26.7053466069166));
#16735=CARTESIAN_POINT('Ctrl Pts',(-3.41609195539438,-8.14886944786305,
26.7064067422891));
#16736=CARTESIAN_POINT('Ctrl Pts',(-3.4079966835452,-8.14527184999125,26.7074398061815));
#16737=CARTESIAN_POINT('Ctrl Pts',(-3.40023150406736,-8.14104782397265,
26.7084282556346));
#16738=CARTESIAN_POINT('Ctrl Pts',(-3.39246811568572,-8.13682477225695,
26.7094164770946));
#16739=CARTESIAN_POINT('Ctrl Pts',(-3.38503564701794,-8.1319760772694,26.7103601046942));
#16740=CARTESIAN_POINT('Ctrl Pts',(-3.37806803706356,-8.1265995263102,26.7112416076109));
#16741=CARTESIAN_POINT('Ctrl Pts',(-3.37708082062299,-8.1258377414894,26.7113665046957));
#16742=CARTESIAN_POINT('Ctrl Pts',(-3.37610288379039,-8.12506542754179,
26.7114901546231));
#16743=CARTESIAN_POINT('Ctrl Pts',(-3.37513455251967,-8.12428292690353,
26.711612507529));
#16744=CARTESIAN_POINT('Ctrl Pts',(-3.3682119411705,-8.118688820875,26.712487209855));
#16745=CARTESIAN_POINT('Ctrl Pts',(-3.36168781356213,-8.11249393562155,
26.7133072646934));
#16746=CARTESIAN_POINT('Ctrl Pts',(-3.35569748527791,-8.10579924528163,
26.714059519658));
#16747=CARTESIAN_POINT('Ctrl Pts',(-3.34971123657186,-8.09910911420979,
26.7148112623164));
#16748=CARTESIAN_POINT('Ctrl Pts',(-3.34425883274771,-8.09192063556458,
26.7154952974168));
#16749=CARTESIAN_POINT('Ctrl Pts',(-3.33943828806449,-8.08437098787273,
26.7160984994262));
#16750=CARTESIAN_POINT('Ctrl Pts',(-3.33892431005329,-8.08356602636715,
26.7161628142681));
#16751=CARTESIAN_POINT('Ctrl Pts',(-3.33841747458821,-8.08275698612942,
26.7162262101724));
#16752=CARTESIAN_POINT('Ctrl Pts',(-3.33791787059189,-8.08194405158577,
26.7162886712293));
#16753=CARTESIAN_POINT('Ctrl Pts',(-3.33371986579937,-8.07511323530855,
26.7168135105385));
#16754=CARTESIAN_POINT('Ctrl Pts',(-3.32998291026763,-8.06791865523384,
26.7172788087242));
#16755=CARTESIAN_POINT('Ctrl Pts',(-3.32679079649677,-8.06048971401084,
26.7176763915555));
#16756=CARTESIAN_POINT('Ctrl Pts',(-3.32554599178153,-8.05759270540544,
26.7178314339564));
#16757=CARTESIAN_POINT('Ctrl Pts',(-3.32438356470384,-8.05466035674258,
26.7179761788316));
#16758=CARTESIAN_POINT('Ctrl Pts',(-3.32330655676031,-8.05170130173715,
26.7181101414338));
#16759=CARTESIAN_POINT('Origin',(0.,-73.5076,0.));
#16760=CARTESIAN_POINT('Origin',(-6.74379561169036,-6.30137626259123,27.4319999999997));
#16761=CARTESIAN_POINT('',(-6.74379561169136,-5.94049664112042,25.1902468135092));
#16762=CARTESIAN_POINT('',(-6.74379561169036,-5.94049664112042,27.4319999999997));
#16763=CARTESIAN_POINT('',(-7.08291152897955,-6.17794816273249,25.0970053602106));
#16764=CARTESIAN_POINT('',(-7.08291152897855,-6.17794816273248,27.4319999999999));
#16765=CARTESIAN_POINT('Ctrl Pts',(-7.08291152897862,-6.17794816273283,
25.0970053602107));
#16766=CARTESIAN_POINT('Ctrl Pts',(-7.08104300930754,-6.17281444712872,
25.097532696414));
#16767=CARTESIAN_POINT('Ctrl Pts',(-7.07905756900056,-6.167722445671,25.0980928053834));
#16768=CARTESIAN_POINT('Ctrl Pts',(-7.05845454038074,-6.1182314418709,25.1039021450715));
#16769=CARTESIAN_POINT('Ctrl Pts',(-7.03066953453777,-6.07788933037055,
25.11171205087));
#16770=CARTESIAN_POINT('Ctrl Pts',(-6.96662822236171,-6.0138480181945,25.129554962186));
#16771=CARTESIAN_POINT('Ctrl Pts',(-6.92586636757164,-5.98610461284618,
25.140839531845));
#16772=CARTESIAN_POINT('Ctrl Pts',(-6.83696964035665,-5.94943227002039,
25.1651601116369));
#16773=CARTESIAN_POINT('Ctrl Pts',(-6.78883556964667,-5.94049664112043,
25.1781889613946));
#16774=CARTESIAN_POINT('Ctrl Pts',(-6.74379561169036,-5.94049664112043,
25.1902468135095));
#16775=CARTESIAN_POINT('Origin',(-5.01347837569466,-6.30137626259108,27.432));
#16776=CARTESIAN_POINT('',(-4.67436245840769,-6.42480436244975,25.6549731901092));
#16777=CARTESIAN_POINT('',(-4.67436245840669,-6.42480436244975,27.432));
#16778=CARTESIAN_POINT('',(-5.01347837569577,-5.94049664112041,25.5908645487843));
#16779=CARTESIAN_POINT('',(-5.01347837569466,-5.9404966411204,27.432));
#16780=CARTESIAN_POINT('Ctrl Pts',(-5.01347837569466,-5.94049664112042,
25.5908645487843));
#16781=CARTESIAN_POINT('Ctrl Pts',(-4.96837290012384,-5.94049664112029,
25.5997011133313));
#16782=CARTESIAN_POINT('Ctrl Pts',(-4.92016024486557,-5.94946691485491,
25.6090098512858));
#16783=CARTESIAN_POINT('Ctrl Pts',(-4.8312331997639,-5.98620145616166,25.625935069141));
#16784=CARTESIAN_POINT('Ctrl Pts',(-4.79052235087904,-6.01397143233882,
25.6335577624367));
#16785=CARTESIAN_POINT('Ctrl Pts',(-4.72641696258039,-6.07807682063747,
25.6454547215909));
#16786=CARTESIAN_POINT('Ctrl Pts',(-4.69863423533746,-6.11855329337769,
25.6505458430842));
#16787=CARTESIAN_POINT('Ctrl Pts',(-4.66172292503951,-6.207465804056,25.6572797680378));
#16788=CARTESIAN_POINT('Ctrl Pts',(-4.65259875422399,-6.25590318490456,
25.6589290230511));
#16789=CARTESIAN_POINT('Ctrl Pts',(-4.65259875422399,-6.30137626259109,
25.6589290230511));
#16790=CARTESIAN_POINT('Ctrl Pts',(-4.65259875422399,-6.34178958168154,
25.6589290230511));
#16791=CARTESIAN_POINT('Ctrl Pts',(-4.65972783943132,-6.38459607727283,
25.6576396327137));
#16792=CARTESIAN_POINT('Ctrl Pts',(-4.67436245840677,-6.42480436245008,
25.6549731901091));
#16793=CARTESIAN_POINT('Origin',(-5.93739595998544,-6.66225588406189,27.432));
#16794=CARTESIAN_POINT('',(-5.78088092123807,-6.71922269938132,25.4285023065114));
#16795=CARTESIAN_POINT('',(-5.78088092123707,-6.71922269938132,27.432));
#16796=CARTESIAN_POINT('',(-5.93739595998644,-6.49569605876776,25.3924130990367));
#16797=CARTESIAN_POINT('Ctrl Pts',(-5.93739595998544,-6.49569605876776,
25.3924130990367));
#16798=CARTESIAN_POINT('Ctrl Pts',(-5.91660446115548,-6.49569605876764,
25.3972746835058));
#16799=CARTESIAN_POINT('Ctrl Pts',(-5.89437223799509,-6.49982272731183,
25.4024432462527));
#16800=CARTESIAN_POINT('Ctrl Pts',(-5.85333291696584,-6.51676428301931,
25.4119314812701));
#16801=CARTESIAN_POINT('Ctrl Pts',(-5.83452470904968,-6.52957597112021,
25.416252063977));
#16802=CARTESIAN_POINT('Ctrl Pts',(-5.80494303836512,-6.55915764180477,
25.423024541048));
#16803=CARTESIAN_POINT('Ctrl Pts',(-5.7921175678169,-6.57781300603602,25.4259464613991));
#16804=CARTESIAN_POINT('Ctrl Pts',(-5.77506551799621,-6.61884921235002,
25.4298254060282));
#16805=CARTESIAN_POINT('Ctrl Pts',(-5.7708361346913,-6.64122876082625,25.4307837882422));
#16806=CARTESIAN_POINT('Ctrl Pts',(-5.7708361346913,-6.66225588406189,25.4307837882422));
#16807=CARTESIAN_POINT('Ctrl Pts',(-5.7708361346913,-6.68091969526821,25.4307837882422));
#16808=CARTESIAN_POINT('Ctrl Pts',(-5.77413148426649,-6.7006787737105,25.4300367142773));
#16809=CARTESIAN_POINT('Ctrl Pts',(-5.78088092123727,-6.71922269938161,
25.4285023065114));
#16810=CARTESIAN_POINT('',(-5.93739595998544,-6.49569605876778,27.432));
#16811=CARTESIAN_POINT('Origin',(-4.90224098782854,-7.05089547641508,27.432));
#16812=CARTESIAN_POINT('',(-4.90224098782954,-7.05089547641508,25.6124061164709));
#16813=CARTESIAN_POINT('',(-4.90224098782854,-7.05089547641508,27.432));
#16814=CARTESIAN_POINT('Origin',(-0.142541304290903,6.02627364624958,-186.976025339984));
#16815=CARTESIAN_POINT('Origin',(-5.90159993959383,-7.05089547641508,27.432));
#16816=CARTESIAN_POINT('',(-5.90159993959483,-7.05089547641508,25.4007565228039));
#16817=CARTESIAN_POINT('',(-5.90159993959383,-7.05089547641508,27.432));
#16818=CARTESIAN_POINT('Origin',(0.,-7.05089547641508,0.));
#16819=CARTESIAN_POINT('Origin',(-5.78088092123707,-6.71922269938132,27.432));
#16820=CARTESIAN_POINT('Origin',(0.000357755259142722,9.16460077541064,
-0.00155622773117425));
#16821=CARTESIAN_POINT('Origin',(-6.08257690813685,-6.66225588406217,27.432));
#16822=CARTESIAN_POINT('',(-6.08257690813785,-6.49569605876776,25.3580277611328));
#16823=CARTESIAN_POINT('',(-6.08257690813685,-6.49569605876778,27.432));
#16824=CARTESIAN_POINT('',(-6.23909194688643,-6.60528906874267,25.3199732514885));
#16825=CARTESIAN_POINT('Ctrl Pts',(-6.2390919468855,-6.605289068743,25.3199732514884));
#16826=CARTESIAN_POINT('Ctrl Pts',(-6.2382913212058,-6.60308936776659,25.320170533578));
#16827=CARTESIAN_POINT('Ctrl Pts',(-6.23744394144666,-6.60090617161399,
25.3203793274821));
#16828=CARTESIAN_POINT('Ctrl Pts',(-6.22814005774519,-6.57834529113788,
25.3226706639561));
#16829=CARTESIAN_POINT('Ctrl Pts',(-6.21548718067666,-6.55978310696465,
25.3257824136204));
#16830=CARTESIAN_POINT('Ctrl Pts',(-6.18608172873822,-6.53004368551921,
25.3329813289223));
#16831=CARTESIAN_POINT('Ctrl Pts',(-6.1671952485578,-6.51706294484019,25.3375902197371));
#16832=CARTESIAN_POINT('Ctrl Pts',(-6.12592247862246,-6.49988754535881,
25.3476000423827));
#16833=CARTESIAN_POINT('Ctrl Pts',(-6.10353478744972,-6.49569605876777,
25.3530006385997));
#16834=CARTESIAN_POINT('Ctrl Pts',(-6.08257690813685,-6.49569605876777,
25.3580277611328));
#16835=CARTESIAN_POINT('',(-6.23909194688532,-6.60528906874266,27.432));
#16836=CARTESIAN_POINT('Origin',(-6.08257690813685,-6.49569605876778,27.432));
#16837=CARTESIAN_POINT('Origin',(0.,-6.49569605876775,0.));
#16838=CARTESIAN_POINT('Origin',(-6.7240744959387,-7.937767671096,27.4319999999997));
#16839=CARTESIAN_POINT('Origin',(-0.353497848166984,9.56524818703472,-178.885460376355));
#16840=CARTESIAN_POINT('Origin',(-6.42237850903871,-7.99473448641576,27.432));
#16841=CARTESIAN_POINT('',(-6.42237850903971,-8.16129431170975,25.2741046936271));
#16842=CARTESIAN_POINT('',(-6.42237850903871,-8.16129431170974,27.432));
#16843=CARTESIAN_POINT('',(-6.26586347029157,-8.05170130173512,25.3133614668116));
#16844=CARTESIAN_POINT('Ctrl Pts',(-6.26586347029067,-8.05170130173544,
25.3133614668115));
#16845=CARTESIAN_POINT('Ctrl Pts',(-6.26666175963764,-8.05389458369041,
25.3131638647639));
#16846=CARTESIAN_POINT('Ctrl Pts',(-6.2675065242362,-8.05607144011045,25.3129547499276));
#16847=CARTESIAN_POINT('Ctrl Pts',(-6.27680192589968,-8.07861962563518,
25.3106526123453));
#16848=CARTESIAN_POINT('Ctrl Pts',(-6.28944590071834,-8.09717495685232,
25.3075167876254));
#16849=CARTESIAN_POINT('Ctrl Pts',(-6.31885565754281,-8.12693847586876,
25.3001900087931));
#16850=CARTESIAN_POINT('Ctrl Pts',(-6.33776601888878,-8.13993184886486,
25.2954640131616));
#16851=CARTESIAN_POINT('Ctrl Pts',(-6.37905917743032,-8.15711175159354,
25.2850817756012));
#16852=CARTESIAN_POINT('Ctrl Pts',(-6.40144336680644,-8.16129431170975,
25.2794245025455));
#16853=CARTESIAN_POINT('Ctrl Pts',(-6.42237850903871,-8.16129431170975,
25.274104693627));
#16854=CARTESIAN_POINT('',(-6.26586347029057,-8.05170130173512,27.432));
#16855=CARTESIAN_POINT('Origin',(-6.42237850903871,-8.16129431170974,27.432));
#16856=CARTESIAN_POINT('Origin',(0.,-8.16129431170914,0.));
#16857=CARTESIAN_POINT('Origin',(-5.76115980548519,-8.35561410788657,27.432));
#16858=CARTESIAN_POINT('',(-5.76115980548619,-8.71649372935709,25.4329776367897));
#16859=CARTESIAN_POINT('',(-5.76115980548519,-8.71649372935708,27.432));
#16860=CARTESIAN_POINT('',(-5.42204388819834,-8.47904220774522,25.5074254649943));
#16861=CARTESIAN_POINT('',(-5.42204388819734,-8.47904220774522,27.432));
#16862=CARTESIAN_POINT('Ctrl Pts',(-5.42204388819745,-8.47904220774555,
25.5074254649943));
#16863=CARTESIAN_POINT('Ctrl Pts',(-5.42378775715849,-8.48383344833847,
25.5070547755237));
#16864=CARTESIAN_POINT('Ctrl Pts',(-5.42563372783266,-8.48858909570021,
25.5066621960722));
#16865=CARTESIAN_POINT('Ctrl Pts',(-5.44584097252921,-8.5375458474019,25.5023622137516));
#16866=CARTESIAN_POINT('Ctrl Pts',(-5.47332200354155,-8.57784090317021,
25.4964918701779));
#16867=CARTESIAN_POINT('Ctrl Pts',(-5.53714217718116,-8.64225062380014,
25.4827091277389));
#16868=CARTESIAN_POINT('Ctrl Pts',(-5.57804053302837,-8.67032322158444,
25.4738075455107));
#16869=CARTESIAN_POINT('Ctrl Pts',(-5.66739282991667,-8.7074411225608,25.4540775822922));
#16870=CARTESIAN_POINT('Ctrl Pts',(-5.7158423859449,-8.7164937293571,25.44324308426));
#16871=CARTESIAN_POINT('Ctrl Pts',(-5.76115980548519,-8.7164937293571,25.4329776367897));
#16872=CARTESIAN_POINT('Origin',(-7.08291152897855,-6.17794816273248,27.4319999999999));
#16873=CARTESIAN_POINT('Origin',(0.,13.2821913271337,0.));
#16874=CARTESIAN_POINT('Origin',(-7.49147704148101,-8.71649372935708,27.4319999999996));
#16875=CARTESIAN_POINT('Origin',(0.,-8.71649372935708,0.));
#16876=CARTESIAN_POINT('Origin',(-6.10367600169937,-7.60609489406241,27.432));
#16877=CARTESIAN_POINT('',(-6.10367600170036,-7.60609489406241,25.3529574812103));
#16878=CARTESIAN_POINT('',(-6.10367600169937,-7.60609489406241,27.432));
#16879=CARTESIAN_POINT('Origin',(0.0007158713098665,9.16558435647346,-0.00293390760594203));
#16880=CARTESIAN_POINT('Origin',(-5.10431704993408,-7.60609489406241,27.432));
#16881=CARTESIAN_POINT('',(-5.10431704993508,-7.60609489406241,25.572900915452));
#16882=CARTESIAN_POINT('',(-5.10431704993408,-7.60609489406241,27.432));
#16883=CARTESIAN_POINT('Origin',(0.,-7.60609489406241,0.));
#16884=CARTESIAN_POINT('Origin',(-5.42204388819734,-8.47904220774522,27.432));
#16885=CARTESIAN_POINT('Origin',(-0.189283519094631,5.89784964622213,-184.941227254179));
#16886=CARTESIAN_POINT('Origin',(-5.01347837569466,-5.94049664112042,27.432));
#16887=CARTESIAN_POINT('Origin',(0.,-5.94049664112037,0.));
#16888=CARTESIAN_POINT('Origin',(0.,-73.5076,0.));
#16889=CARTESIAN_POINT('Origin',(7.49781464960508,-6.30137626259116,27.432));
#16890=CARTESIAN_POINT('',(7.49781464960408,-5.94049664112042,24.9761904472629));
#16891=CARTESIAN_POINT('',(7.49781464960508,-5.94049664112042,27.432));
#16892=CARTESIAN_POINT('',(7.158698732316,-6.17794816273246,25.0754929410708));
#16893=CARTESIAN_POINT('',(7.158698732317,-6.17794816273246,27.4319999999997));
#16894=CARTESIAN_POINT('Ctrl Pts',(7.15869873231689,-6.17794816273275,25.0754929410711));
#16895=CARTESIAN_POINT('Ctrl Pts',(7.16040494095542,-6.17326039302549,25.0750058426261));
#16896=CARTESIAN_POINT('Ctrl Pts',(7.16220853284073,-6.16860767021153,25.0744907546918));
#16897=CARTESIAN_POINT('Ctrl Pts',(7.18225441450641,-6.1199143069236,25.068763262829));
#16898=CARTESIAN_POINT('Ctrl Pts',(7.20951435418224,-6.07983631592374,25.0609509572572));
#16899=CARTESIAN_POINT('Ctrl Pts',(7.27313274533492,-6.01518591740008,25.0425637940817));
#16900=CARTESIAN_POINT('Ctrl Pts',(7.31425703075933,-5.98689326888735,25.0306041101757));
#16901=CARTESIAN_POINT('Ctrl Pts',(7.40392986412281,-5.94955443337069,25.0042260548048));
#16902=CARTESIAN_POINT('Ctrl Pts',(7.45247198035741,-5.94049664112041,24.989802248088));
#16903=CARTESIAN_POINT('Ctrl Pts',(7.49781464960508,-5.94049664112041,24.9761904472629));
#16904=CARTESIAN_POINT('Origin',(8.22877293383528,-6.30137626259123,27.4319999999996));
#16905=CARTESIAN_POINT('',(8.56788885112282,-6.42480436244998,24.629628385596));
#16906=CARTESIAN_POINT('',(8.56788885112347,-6.42480436244998,27.4319999999996));
#16907=CARTESIAN_POINT('',(8.22877293383474,-5.94049664112041,24.7449916100438));
#16908=CARTESIAN_POINT('',(8.22877293383528,-5.9404966411204,27.4319999999996));
#16909=CARTESIAN_POINT('Ctrl Pts',(8.22877293383528,-5.94049664112042,24.7449916100443));
#16910=CARTESIAN_POINT('Ctrl Pts',(8.27366797515212,-5.94049664112037,24.7300620797913));
#16911=CARTESIAN_POINT('Ctrl Pts',(8.32169951269488,-5.94936937943643,24.7139400541798));
#16912=CARTESIAN_POINT('Ctrl Pts',(8.41058956422228,-5.98596081038067,24.6838307189797));
#16913=CARTESIAN_POINT('Ctrl Pts',(8.45144666045887,-6.01368913414672,24.6698509296916));
#16914=CARTESIAN_POINT('Ctrl Pts',(8.51547225051043,-6.07771472419829,24.6478225644119));
#16915=CARTESIAN_POINT('Ctrl Pts',(8.54326072818976,-6.11793440898385,24.6381897785089));
#16916=CARTESIAN_POINT('Ctrl Pts',(8.58035961940092,-6.20682316665666,24.6252944801456));
#16917=CARTESIAN_POINT('Ctrl Pts',(8.5896525553061,-6.25550166682477,24.6220466809099));
#16918=CARTESIAN_POINT('Ctrl Pts',(8.5896525553061,-6.30137626259124,24.6220466809099));
#16919=CARTESIAN_POINT('Ctrl Pts',(8.5896525553061,-6.34190862553465,24.6220466809099));
#16920=CARTESIAN_POINT('Ctrl Pts',(8.58247260949824,-6.38473581562443,24.6245551453984));
#16921=CARTESIAN_POINT('Ctrl Pts',(8.56788885112337,-6.42480436245012,24.6296283855964));
#16922=CARTESIAN_POINT('Origin',(7.30485534954484,-6.66225588406186,27.4319999999997));
#16923=CARTESIAN_POINT('',(7.46137038829209,-6.71922269938127,24.9871019869548));
#16924=CARTESIAN_POINT('',(7.46137038829309,-6.71922269938127,27.432));
#16925=CARTESIAN_POINT('',(7.30485534954384,-6.49569605876775,25.0333058563985));
#16926=CARTESIAN_POINT('Ctrl Pts',(7.30485534954484,-6.49569605876775,25.0333058563987));
#16927=CARTESIAN_POINT('Ctrl Pts',(7.32583110676964,-6.49569605876764,25.0271850158972));
#16928=CARTESIAN_POINT('Ctrl Pts',(7.34825401952324,-6.49989204958677,25.0206101300395));
#16929=CARTESIAN_POINT('Ctrl Pts',(7.3896338158284,-6.51714724083042,25.0084206171891));
#16930=CARTESIAN_POINT('Ctrl Pts',(7.40859274088765,-6.53020161408073,25.0028060878397));
#16931=CARTESIAN_POINT('Ctrl Pts',(7.43792386108939,-6.56001849076957,24.9940958200722));
#16932=CARTESIAN_POINT('Ctrl Pts',(7.45050115658508,-6.57850457858891,24.9903463704326));
#16933=CARTESIAN_POINT('Ctrl Pts',(7.46724465195333,-6.61918812648831,24.9853488902099));
#16934=CARTESIAN_POINT('Ctrl Pts',(7.47141517483894,-6.64138374163587,24.9841003252662));
#16935=CARTESIAN_POINT('Ctrl Pts',(7.47141517483894,-6.66225588406186,24.9841003252662));
#16936=CARTESIAN_POINT('Ctrl Pts',(7.47141517483894,-6.68094317211439,24.9841003252662));
#16937=CARTESIAN_POINT('Ctrl Pts',(7.46810980382901,-6.70070630737614,24.9850895376704));
#16938=CARTESIAN_POINT('Ctrl Pts',(7.46137038829298,-6.71922269938158,24.9871019869549));
#16939=CARTESIAN_POINT('',(7.30485534954484,-6.49569605876775,27.4319999999997));
#16940=CARTESIAN_POINT('Origin',(7.73378213538489,-8.71649372935708,27.432));
#16941=CARTESIAN_POINT('',(7.73378213538389,-8.71649372935708,24.9041347502815));
#16942=CARTESIAN_POINT('',(7.73378213538489,-8.71649372935708,27.432));
#16943=CARTESIAN_POINT('Origin',(0.,-29.9648855133081,0.));
#16944=CARTESIAN_POINT('Origin',(6.73442318361961,-8.71649372935708,27.432));
#16945=CARTESIAN_POINT('',(6.73442318361861,-8.71649372935708,25.1927540805229));
#16946=CARTESIAN_POINT('',(6.73442318361961,-8.71649372935708,27.432));
#16947=CARTESIAN_POINT('Origin',(0.,-8.71649372935708,0.));
#16948=CARTESIAN_POINT('Origin',(7.46137038829309,-6.71922269938127,27.432));
#16949=CARTESIAN_POINT('Origin',(0.,-27.2191693594009,0.));
#16950=CARTESIAN_POINT('Origin',(7.15967440139342,-6.66225588406219,27.4319999999997));
#16951=CARTESIAN_POINT('',(7.15967440139242,-6.49569605876775,25.0752143808144));
#16952=CARTESIAN_POINT('',(7.15967440139342,-6.49569605876775,27.4319999999997));
#16953=CARTESIAN_POINT('',(7.00315936264384,-6.60528906874269,25.1193764396963));
#16954=CARTESIAN_POINT('Ctrl Pts',(7.00315936264473,-6.60528906874299,25.1193764396966));
#16955=CARTESIAN_POINT('Ctrl Pts',(7.00395000043857,-6.60311680925744,25.1191560137444));
#16956=CARTESIAN_POINT('Ctrl Pts',(7.0047862037078,-6.60096088559641,25.1189228759655));
#16957=CARTESIAN_POINT('Ctrl Pts',(7.01404818052029,-6.57846633092419,25.1163394388245));
#16958=CARTESIAN_POINT('Ctrl Pts',(7.02664725380163,-6.55995591519301,25.1128207277713));
#16959=CARTESIAN_POINT('Ctrl Pts',(7.05601462041678,-6.53014425969475,25.1045855181729));
#16960=CARTESIAN_POINT('Ctrl Pts',(7.07497015810655,-6.51710661368603,25.0992546425158));
#16961=CARTESIAN_POINT('Ctrl Pts',(7.11632795690618,-6.49987999375941,25.0875594939658));
#16962=CARTESIAN_POINT('Ctrl Pts',(7.13873197918201,-6.49569605876774,25.0811940275659));
#16963=CARTESIAN_POINT('Ctrl Pts',(7.15967440139342,-6.49569605876774,25.0752143808146));
#16964=CARTESIAN_POINT('',(7.00315936264484,-6.60528906874269,27.4319999999997));
#16965=CARTESIAN_POINT('Origin',(7.15967440139342,-6.49569605876775,27.4319999999997));
#16966=CARTESIAN_POINT('Origin',(0.,-6.49569605876775,0.));
#16967=CARTESIAN_POINT('Origin',(6.24576506649965,-5.94049664112042,27.432));
#16968=CARTESIAN_POINT('',(6.24576506649865,-5.94049664112042,25.3183279959769));
#16969=CARTESIAN_POINT('',(6.24576506649965,-5.94049664112042,27.432));
#16970=CARTESIAN_POINT('',(5.23538475597085,-8.71649372935708,25.5463903562659));
#16971=CARTESIAN_POINT('',(5.23538475597185,-8.71649372935708,27.432));
#16972=CARTESIAN_POINT('Origin',(0.,-23.1005951285458,0.));
#16973=CARTESIAN_POINT('Origin',(7.24512401826494,-5.94049664112042,27.4319999999997));
#16974=CARTESIAN_POINT('',(7.24512401826394,-5.94049664112042,25.0506585090637));
#16975=CARTESIAN_POINT('',(7.24512401826494,-5.94049664112042,27.4319999999997));
#16976=CARTESIAN_POINT('Origin',(0.,-5.94049664112042,0.));
#16977=CARTESIAN_POINT('Origin',(7.158698732317,-6.17794816273246,27.4319999999997));
#16978=CARTESIAN_POINT('Origin',(0.00220247838234822,-25.8402585961412,
0.00767166622851256));
#16979=CARTESIAN_POINT('Origin',(6.23474370773713,-8.71649372935708,27.432));
#16980=CARTESIAN_POINT('',(6.23474370773613,-8.71649372935708,25.3210443046216));
#16981=CARTESIAN_POINT('',(6.23474370773713,-8.71649372935708,27.432));
#16982=CARTESIAN_POINT('Origin',(0.,-25.8463112824522,0.));
#16983=CARTESIAN_POINT('Origin',(5.23538475597185,-8.71649372935708,27.432));
#16984=CARTESIAN_POINT('Origin',(0.,-8.71649372935708,0.));
#16985=CARTESIAN_POINT('Origin',(8.22877293383528,-5.94049664112042,27.4319999999996));
#16986=CARTESIAN_POINT('Origin',(0.,-5.94049664112042,0.));
#16987=CARTESIAN_POINT('Origin',(0.,-73.5076,0.));
#16988=CARTESIAN_POINT('Origin',(-0.779753153286711,-5.10769751464934,27.432));
#16989=CARTESIAN_POINT('',(-0.779753153287141,-5.10769751464934,26.0656728053914));
#16990=CARTESIAN_POINT('',(-0.779753153286711,-5.10769751464934,27.432));
#16991=CARTESIAN_POINT('',(-2.09324755697336,-8.71649372935708,25.9931842690153));
#16992=CARTESIAN_POINT('',(-2.09324755697293,-8.71649372935708,27.4319999999996));
#16993=CARTESIAN_POINT('Origin',(0.,-2.96534333324559,0.));
#16994=CARTESIAN_POINT('Origin',(0.219605798478462,-5.10769751464934,27.432));
#16995=CARTESIAN_POINT('',(0.219605798478031,-5.10769751464934,26.0764086306197));
#16996=CARTESIAN_POINT('',(0.219605798478462,-5.10769751464934,27.432));
#16997=CARTESIAN_POINT('Origin',(0.,-5.10769751464934,0.));
#16998=CARTESIAN_POINT('Origin',(-1.09388860520765,-8.71649372935708,27.432));
#16999=CARTESIAN_POINT('',(-1.09388860520808,-8.71649372935708,26.0543800827648));
#17000=CARTESIAN_POINT('',(-1.09388860520765,-8.71649372935708,27.432));
#17001=CARTESIAN_POINT('Origin',(-4.73278305357025E-5,-5.71118949475327,
-196.733954044368));
#17002=CARTESIAN_POINT('Origin',(-2.09324755697293,-8.71649372935708,27.4319999999996));
#17003=CARTESIAN_POINT('Origin',(0.,-8.71649372935708,0.));
#17004=CARTESIAN_POINT('Origin',(0.,-73.5076,0.));
#17005=CARTESIAN_POINT('Origin',(4.06060244911334,-6.60528906874484,53.8479999999997));
#17006=CARTESIAN_POINT('',(4.06060244911333,-6.60528906874484,25.7592473012705));
#17007=CARTESIAN_POINT('Origin',(0.0722104791913641,-17.5633056413909,-190.547537117087));
#17008=CARTESIAN_POINT('',(4.06060244911444,-6.60528906874484,26.6160343355322));
#17009=CARTESIAN_POINT('Origin',(0.0677399631732983,-17.5755885780715,-197.134834438701));
#17010=CARTESIAN_POINT('',(4.06060244911334,-6.60528906874484,53.8479999999997));
#17011=CARTESIAN_POINT('Origin',(4.21711748786159,-6.66225588406422,53.848));
#17012=CARTESIAN_POINT('',(4.21711748786158,-6.49569605877014,25.7340870028712));
#17013=CARTESIAN_POINT('Ctrl Pts',(4.06060244911336,-6.60528906874485,25.7592473012705));
#17014=CARTESIAN_POINT('Ctrl Pts',(4.06357955182199,-6.59710954627748,25.7587780006575));
#17015=CARTESIAN_POINT('Ctrl Pts',(4.06721997470441,-6.58911531508258,25.7582015133841));
#17016=CARTESIAN_POINT('Ctrl Pts',(4.07146638853431,-6.58146026124499,25.7575301233568));
#17017=CARTESIAN_POINT('Ctrl Pts',(4.07571480311339,-6.57380160063629,25.7568584169959));
#17018=CARTESIAN_POINT('Ctrl Pts',(4.08056923939063,-6.56648339411849,25.7560917184307));
#17019=CARTESIAN_POINT('Ctrl Pts',(4.08592700394529,-6.55963409138937,25.7552423289387));
#17020=CARTESIAN_POINT('Ctrl Pts',(4.08666507444826,-6.55869055080287,25.7551253194428));
#17021=CARTESIAN_POINT('Ctrl Pts',(4.08741263481808,-6.55775585629798,25.755006740718));
#17022=CARTESIAN_POINT('Ctrl Pts',(4.0881693599018,-6.55683029088278,25.7548866249225));
#17023=CARTESIAN_POINT('Ctrl Pts',(4.09371519313907,-6.55004707257361,25.7540063287818));
#17024=CARTESIAN_POINT('Ctrl Pts',(4.0998309663577,-6.54366587591398,25.7530320575225));
#17025=CARTESIAN_POINT('Ctrl Pts',(4.10641013147035,-6.53781289855337,25.7519828577906));
#17026=CARTESIAN_POINT('Ctrl Pts',(4.11299286548831,-6.53195674621208,25.7509330889144));
#17027=CARTESIAN_POINT('Ctrl Pts',(4.12003866230595,-6.52663010445927,25.7498083102528));
#17028=CARTESIAN_POINT('Ctrl Pts',(4.12740681314746,-6.52191996476938,25.7486275994646));
#17029=CARTESIAN_POINT('Ctrl Pts',(4.12825534516983,-6.52137753500068,25.7484916262829));
#17030=CARTESIAN_POINT('Ctrl Pts',(4.12910812389234,-6.52084323219908,25.7483549113116));
#17031=CARTESIAN_POINT('Ctrl Pts',(4.12996491394956,-6.5203171498776,25.7482174836882));
#17032=CARTESIAN_POINT('Ctrl Pts',(4.13789954422865,-6.51544516439862,25.7469447828991));
#17033=CARTESIAN_POINT('Ctrl Pts',(4.14629235146124,-6.51121383586506,25.7455936204303));
#17034=CARTESIAN_POINT('Ctrl Pts',(4.1549823764977,-6.50771979333526,25.7441911047125));
#17035=CARTESIAN_POINT('Ctrl Pts',(4.16367240153416,-6.50422575080547,25.7427885889946));
#17036=CARTESIAN_POINT('Ctrl Pts',(4.17265845008949,-6.50146947482356,25.7413347200278));
#17037=CARTESIAN_POINT('Ctrl Pts',(4.18175748826421,-6.4994927253628,25.7398566062428));
#17038=CARTESIAN_POINT('Ctrl Pts',(4.18984486336934,-6.49773575786018,25.7385428343475));
#17039=CARTESIAN_POINT('Ctrl Pts',(4.1981209728453,-6.49657345662428,25.7371941175886));
#17040=CARTESIAN_POINT('Ctrl Pts',(4.20643201854385,-6.49603916965965,25.7358357408497));
#17041=CARTESIAN_POINT('Ctrl Pts',(4.20999170079618,-6.49581033060682,25.7352539380604));
#17042=CARTESIAN_POINT('Ctrl Pts',(4.21355765229966,-6.49569605877015,25.7346703631746));
#17043=CARTESIAN_POINT('Ctrl Pts',(4.21711748786158,-6.49569605877015,25.7340870028712));
#17044=CARTESIAN_POINT('',(4.21711748786258,-6.49569605877014,26.5916847170984));
#17045=CARTESIAN_POINT('Ctrl Pts',(4.21711748786258,-6.49569605877015,26.5916847170984));
#17046=CARTESIAN_POINT('Ctrl Pts',(4.20828491160098,-6.4956960587701,26.593085456172));
#17047=CARTESIAN_POINT('Ctrl Pts',(4.19939227477984,-6.49640297706072,26.5944906400047));
#17048=CARTESIAN_POINT('Ctrl Pts',(4.19060659306914,-6.49781942868009,26.5958748669163));
#17049=CARTESIAN_POINT('Ctrl Pts',(4.1818221174255,-6.49923568585404,26.5972589038061));
#17050=CARTESIAN_POINT('Ctrl Pts',(4.17314565503541,-6.50136113209613,26.5986219895282));
#17051=CARTESIAN_POINT('Ctrl Pts',(4.16473688918655,-6.50414690808741,26.5999387328621));
#17052=CARTESIAN_POINT('Ctrl Pts',(4.16365033292661,-6.50450687795653,26.600108878605));
#17053=CARTESIAN_POINT('Ctrl Pts',(4.16256822343775,-6.50487780576759,26.6002782505664));
#17054=CARTESIAN_POINT('Ctrl Pts',(4.16149088206754,-6.50525952700513,26.6004467939636));
#17055=CARTESIAN_POINT('Ctrl Pts',(4.15321329298771,-6.50819242426016,26.601741771603));
#17056=CARTESIAN_POINT('Ctrl Pts',(4.14510753429725,-6.5118058732504,26.6030046484746));
#17057=CARTESIAN_POINT('Ctrl Pts',(4.13733196734654,-6.51604902335606,26.6042136988607));
#17058=CARTESIAN_POINT('Ctrl Pts',(4.12955920710659,-6.52029064183128,26.6054223128214));
#17059=CARTESIAN_POINT('Ctrl Pts',(4.12211738272986,-6.52516101735553,26.6065771391487));
#17060=CARTESIAN_POINT('Ctrl Pts',(4.11514127341982,-6.53056295680494,26.6076564756432));
#17061=CARTESIAN_POINT('Ctrl Pts',(4.11412286241123,-6.53135156179355,26.6078140431524));
#17062=CARTESIAN_POINT('Ctrl Pts',(4.11311432141515,-6.53215142332433,26.6079700018393));
#17063=CARTESIAN_POINT('Ctrl Pts',(4.11211600972177,-6.53296216808992,26.6081242841838));
#17064=CARTESIAN_POINT('Ctrl Pts',(4.10521380194572,-6.5385675605365,26.6091909738808));
#17065=CARTESIAN_POINT('Ctrl Pts',(4.09870823531688,-6.54477363258281,26.6101917042861));
#17066=CARTESIAN_POINT('Ctrl Pts',(4.09273527158219,-6.55148025644056,26.6111100482618));
#17067=CARTESIAN_POINT('Ctrl Pts',(4.08676730344874,-6.55818127108653,26.6120276241632));
#17068=CARTESIAN_POINT('Ctrl Pts',(4.08133182562738,-6.56538122965243,26.6128629513882));
#17069=CARTESIAN_POINT('Ctrl Pts',(4.07652768479288,-6.57294360789183,26.6135996439821));
#17070=CARTESIAN_POINT('Ctrl Pts',(4.07597749727183,-6.57380967870035,26.6136840126728));
#17071=CARTESIAN_POINT('Ctrl Pts',(4.07543554355856,-6.57468047127657,26.6137670877056));
#17072=CARTESIAN_POINT('Ctrl Pts',(4.07490193496067,-6.57555575767978,26.613848844468));
#17073=CARTESIAN_POINT('Ctrl Pts',(4.07075920680105,-6.58235113849763,26.61448357195));
#17074=CARTESIAN_POINT('Ctrl Pts',(4.06707017876919,-6.58950648258038,26.6150467071816));
#17075=CARTESIAN_POINT('Ctrl Pts',(4.0639186378629,-6.59689314421136,26.6155280483911));
#17076=CARTESIAN_POINT('Ctrl Pts',(4.06273725395373,-6.59966210182697,26.6157084835422));
#17077=CARTESIAN_POINT('Ctrl Pts',(4.06163095039427,-6.60246328469969,26.6158774250486));
#17078=CARTESIAN_POINT('Ctrl Pts',(4.06060244911349,-6.60528906874449,26.6160343355322));
#17079=CARTESIAN_POINT('',(4.21711748786159,-6.49569605877014,53.848));
#17080=CARTESIAN_POINT('Origin',(4.362298436013,-6.49569605877014,53.848));
#17081=CARTESIAN_POINT('',(4.3622984360131,-6.49569605877014,25.7098748758708));
#17082=CARTESIAN_POINT('Origin',(0.,-6.49569605877014,0.));
#17083=CARTESIAN_POINT('',(4.3622984360141,-6.49569605877014,26.5682541457874));
#17084=CARTESIAN_POINT('Origin',(0.,-6.49569605877014,0.));
#17085=CARTESIAN_POINT('',(4.362298436013,-6.49569605877014,53.848));
#17086=CARTESIAN_POINT('Origin',(4.362298436013,-6.66225588406443,53.848));
#17087=CARTESIAN_POINT('',(4.51881347476146,-6.71922269938386,25.6828276978624));
#17088=CARTESIAN_POINT('Ctrl Pts',(4.362298436013,-6.49569605877016,25.7098748758709));
#17089=CARTESIAN_POINT('Ctrl Pts',(4.38315670073796,-6.49569605877017,25.7063357697482));
#17090=CARTESIAN_POINT('Ctrl Pts',(4.40542597239156,-6.49985083245185,25.7025282572255));
#17091=CARTESIAN_POINT('Ctrl Pts',(4.44646060095889,-6.51682001298565,25.6954615814517));
#17092=CARTESIAN_POINT('Ctrl Pts',(4.46522665832712,-6.52963294250088,25.6922029381666));
#17093=CARTESIAN_POINT('Ctrl Pts',(4.49479796836994,-6.5592042525437,25.6870459257064));
#17094=CARTESIAN_POINT('Ctrl Pts',(4.50762009530804,-6.57788995888562,25.684795872475));
#17095=CARTESIAN_POINT('Ctrl Pts',(4.52464939871756,-6.6189258441339,25.6818018785314));
#17096=CARTESIAN_POINT('Ctrl Pts',(4.52885826130728,-6.64127535146051,25.681058323729));
#17097=CARTESIAN_POINT('Ctrl Pts',(4.52885826130728,-6.66225588406443,25.681058323729));
#17098=CARTESIAN_POINT('Ctrl Pts',(4.52885826130728,-6.68090716714125,25.681058323729));
#17099=CARTESIAN_POINT('Ctrl Pts',(4.52556867575988,-6.70066293717673,25.6816391413042));
#17100=CARTESIAN_POINT('Ctrl Pts',(4.51881347476144,-6.71922269938384,25.6828276978625));
#17101=CARTESIAN_POINT('',(4.51881347476246,-6.71922269938386,26.5420816964364));
#17102=CARTESIAN_POINT('Ctrl Pts',(4.51881347476156,-6.71922269938352,26.5420816964366));
#17103=CARTESIAN_POINT('Ctrl Pts',(4.52556921448003,-6.70066145705517,26.540931525624));
#17104=CARTESIAN_POINT('Ctrl Pts',(4.52885826130728,-6.68090594219119,26.5403696064879));
#17105=CARTESIAN_POINT('Ctrl Pts',(4.52885826130728,-6.66225588406443,26.5403696064879));
#17106=CARTESIAN_POINT('Ctrl Pts',(4.52885826130728,-6.64127960312279,26.5403696064879));
#17107=CARTESIAN_POINT('Ctrl Pts',(4.52465125693505,-6.6189327342932,26.5410887671925));
#17108=CARTESIAN_POINT('Ctrl Pts',(4.50762392115929,-6.57789676497924,26.5439855072053));
#17109=CARTESIAN_POINT('Ctrl Pts',(4.49480200888133,-6.55920829305509,26.5461626980549));
#17110=CARTESIAN_POINT('Ctrl Pts',(4.465230356677,-6.52963664085077,26.5511529028482));
#17111=CARTESIAN_POINT('Ctrl Pts',(4.44646657496487,-6.51682335174781,26.554305756238));
#17112=CARTESIAN_POINT('Ctrl Pts',(4.40543178750702,-6.49985236868581,26.5611439701303));
#17113=CARTESIAN_POINT('Ctrl Pts',(4.38316012437418,-6.49569605877016,26.5648288205851));
#17114=CARTESIAN_POINT('Ctrl Pts',(4.362298436013,-6.49569605877016,26.5682541457876));
#17115=CARTESIAN_POINT('',(4.51881347476148,-6.71922269938386,53.848));
#17116=CARTESIAN_POINT('Origin',(4.03383092570821,-8.05170130173722,53.8479999999997));
#17117=CARTESIAN_POINT('',(4.03383092570819,-8.05170130173722,25.7634532204158));
#17118=CARTESIAN_POINT('Origin',(0.101474044156332,-18.8557626288544,-188.956505666068));
#17119=CARTESIAN_POINT('',(4.03383092570919,-8.05170130173722,26.6201048845187));
#17120=CARTESIAN_POINT('Origin',(0.0951918157973997,-18.873023285086,-195.59266431425));
#17121=CARTESIAN_POINT('',(4.03383092570821,-8.05170130173722,53.8479999999997));
#17122=CARTESIAN_POINT('Origin',(3.87731588695962,-7.99473448641774,53.8479999999997));
#17123=CARTESIAN_POINT('',(3.87731588695972,-8.16129431171214,25.7874724486617));
#17124=CARTESIAN_POINT('Ctrl Pts',(4.03383092570815,-8.0517013017372,25.7634532204158));
#17125=CARTESIAN_POINT('Ctrl Pts',(4.0308510870507,-8.05988834116217,25.7639197791969));
#17126=CARTESIAN_POINT('Ctrl Pts',(4.02720669388649,-8.0678898123561,25.7644920148041));
#17127=CARTESIAN_POINT('Ctrl Pts',(4.02295503638535,-8.07555164769332,25.7651560204273));
#17128=CARTESIAN_POINT('Ctrl Pts',(4.01870147210573,-8.08321691920169,25.765820323843));
#17129=CARTESIAN_POINT('Ctrl Pts',(4.01384063833169,-8.09054129269105,25.766576479607));
#17130=CARTESIAN_POINT('Ctrl Pts',(4.0084752019622,-8.09739611259885,25.7674105621899));
#17131=CARTESIAN_POINT('Ctrl Pts',(4.00774109221824,-8.09833400277978,25.7675246830385));
#17132=CARTESIAN_POINT('Ctrl Pts',(4.00699759721028,-8.09926315438219,25.7676402626974));
#17133=CARTESIAN_POINT('Ctrl Pts',(4.00624503544365,-8.10018328950851,25.7677572654986));
#17134=CARTESIAN_POINT('Ctrl Pts',(4.00069187405521,-8.1069729765246,25.7686206304295));
#17135=CARTESIAN_POINT('Ctrl Pts',(3.99456714541196,-8.11336021200005,25.7695724944994));
#17136=CARTESIAN_POINT('Ctrl Pts',(3.98797724155297,-8.11921838096502,25.7705923381123));
#17137=CARTESIAN_POINT('Ctrl Pts',(3.98138418369339,-8.12507935371421,25.7716126698337));
#17138=CARTESIAN_POINT('Ctrl Pts',(3.97432633514388,-8.13041003309948,25.7727010461852));
#17139=CARTESIAN_POINT('Ctrl Pts',(3.96694432322261,-8.13512294326212,25.7738369180945));
#17140=CARTESIAN_POINT('Ctrl Pts',(3.96610059906986,-8.13566160347784,25.7739667421282));
#17141=CARTESIAN_POINT('Ctrl Pts',(3.96525266844851,-8.13619224209497,25.7740971866085));
#17142=CARTESIAN_POINT('Ctrl Pts',(3.96440076140843,-8.13671476689475,25.7742282208546));
#17143=CARTESIAN_POINT('Ctrl Pts',(3.95645614382031,-8.14158766912371,25.7754502050934));
#17144=CARTESIAN_POINT('Ctrl Pts',(3.9480511243051,-8.1458194605454,25.7767399859595));
#17145=CARTESIAN_POINT('Ctrl Pts',(3.93934671604597,-8.14931246558992,25.7780701457675));
#17146=CARTESIAN_POINT('Ctrl Pts',(3.93064230778684,-8.15280547063444,25.7794003055754));
#17147=CARTESIAN_POINT('Ctrl Pts',(3.92163970713197,-8.15555919937222,25.7807708443252));
#17148=CARTESIAN_POINT('Ctrl Pts',(3.91252234858113,-8.15753092514472,25.7821543443313));
#17149=CARTESIAN_POINT('Ctrl Pts',(3.90445534406164,-8.1592755006848,25.7833784599279));
#17150=CARTESIAN_POINT('Ctrl Pts',(3.89619905331137,-8.16042890598883,25.7846275267046));
#17151=CARTESIAN_POINT('Ctrl Pts',(3.88790688219187,-8.16095724726018,25.7858777948854));
#17152=CARTESIAN_POINT('Ctrl Pts',(3.88437886592507,-8.16118203719432,25.7864097383796));
#17153=CARTESIAN_POINT('Ctrl Pts',(3.88084449441112,-8.16129431171212,25.7869418993511));
#17154=CARTESIAN_POINT('Ctrl Pts',(3.87731588695972,-8.16129431171212,25.7874724486617));
#17155=CARTESIAN_POINT('',(3.87731588696072,-8.16129431171213,26.6433518445541));
#17156=CARTESIAN_POINT('Ctrl Pts',(3.87731588696072,-8.16129431171212,26.6433518445541));
#17157=CARTESIAN_POINT('Ctrl Pts',(3.88614428340058,-8.16129431171206,26.642067078209));
#17158=CARTESIAN_POINT('Ctrl Pts',(3.89503129273223,-8.16058805711975,26.6407693606194));
#17159=CARTESIAN_POINT('Ctrl Pts',(3.90381004749686,-8.15917363887092,26.6394829677838));
#17160=CARTESIAN_POINT('Ctrl Pts',(3.91258838392764,-8.15775928802335,26.6381966362486));
#17161=CARTESIAN_POINT('Ctrl Pts',(3.92125738913329,-8.15563699578335,26.6369216283882));
#17162=CARTESIAN_POINT('Ctrl Pts',(3.92965771481654,-8.15285630167006,26.6356822167307));
#17163=CARTESIAN_POINT('Ctrl Pts',(3.93074595484405,-8.15249607008471,26.6355216542207));
#17164=CARTESIAN_POINT('Ctrl Pts',(3.93182970914515,-8.15212485671451,26.6353616891047));
#17165=CARTESIAN_POINT('Ctrl Pts',(3.93290865490423,-8.15174282872588,26.6352023741542));
#17166=CARTESIAN_POINT('Ctrl Pts',(3.94119495348593,-8.14880885548981,26.6339788360508));
#17167=CARTESIAN_POINT('Ctrl Pts',(3.94930751592418,-8.14519358015591,26.6327778523995));
#17168=CARTESIAN_POINT('Ctrl Pts',(3.9570881422175,-8.14094858523576,26.6316218956328));
#17169=CARTESIAN_POINT('Ctrl Pts',(3.96486660283085,-8.13670477187865,26.6304662606182));
#17170=CARTESIAN_POINT('Ctrl Pts',(3.97231233191133,-8.13183208384492,26.629355627426));
#17171=CARTESIAN_POINT('Ctrl Pts',(3.97929088004504,-8.12642835942375,26.6283124497289));
#17172=CARTESIAN_POINT('Ctrl Pts',(3.98027734916442,-8.125664503222,26.6281649888868));
#17173=CARTESIAN_POINT('Ctrl Pts',(3.98125453525714,-8.124890103283,26.6280188759339));
#17174=CARTESIAN_POINT('Ctrl Pts',(3.98222211309492,-8.12410549986412,26.6278741742924));
#17175=CARTESIAN_POINT('Ctrl Pts',(3.98913952241355,-8.11849621160921,26.6268396730422));
#17176=CARTESIAN_POINT('Ctrl Pts',(3.99565840681745,-8.11228489434844,26.6258637485756));
#17177=CARTESIAN_POINT('Ctrl Pts',(4.0016428554866,-8.10557211675593,26.6249645833111));
#17178=CARTESIAN_POINT('Ctrl Pts',(4.00762257292549,-8.09886464620143,26.6240661289155));
#17179=CARTESIAN_POINT('Ctrl Pts',(4.01306792322687,-8.09165728059141,26.6232443124004));
#17180=CARTESIAN_POINT('Ctrl Pts',(4.01788016790894,-8.08408692523894,26.6225172730939));
#17181=CARTESIAN_POINT('Ctrl Pts',(4.01841249612992,-8.08324949612565,26.6224368483512));
#17182=CARTESIAN_POINT('Ctrl Pts',(4.01893712080851,-8.08240765464127,26.6223575833667));
#17183=CARTESIAN_POINT('Ctrl Pts',(4.01945394169786,-8.08156160658952,26.6222795026943));
#17184=CARTESIAN_POINT('Ctrl Pts',(4.02361085166389,-8.07475664639822,26.6216514817839));
#17185=CARTESIAN_POINT('Ctrl Pts',(4.02731224868143,-8.06759052728903,26.6210923589572));
#17186=CARTESIAN_POINT('Ctrl Pts',(4.03047424859968,-8.06019204260363,26.6206134768327));
#17187=CARTESIAN_POINT('Ctrl Pts',(4.0316708709816,-8.05739217144747,26.6204322494186));
#17188=CARTESIAN_POINT('Ctrl Pts',(4.03279069714533,-8.05455930622464,26.6202625137303));
#17189=CARTESIAN_POINT('Ctrl Pts',(4.03383092570827,-8.05170130173688,26.6201048845187));
#17190=CARTESIAN_POINT('',(3.87731588695962,-8.16129431171214,53.8479999999997));
#17191=CARTESIAN_POINT('Origin',(3.73213493880821,-8.16129431171214,53.8479999999997));
#17192=CARTESIAN_POINT('Origin',(0.,-8.16129431171214,0.));
#17193=CARTESIAN_POINT('Origin',(0.,-8.16129431171214,0.));
#17194=CARTESIAN_POINT('Origin',(0.,-73.5076,0.));
#17195=CARTESIAN_POINT('Origin',(0.,-73.5076,0.));
#17196=CARTESIAN_POINT('',(3.21678286702033,-6.17794816273248,25.8781688255602));
#17197=CARTESIAN_POINT('Origin',(0.0297153313338341,-14.9343441661834,-193.338348695396));
#17198=CARTESIAN_POINT('',(4.53853459051312,-8.71649372935708,25.679350021924));
#17199=CARTESIAN_POINT('Origin',(0.,-8.71649372935708,0.));
#17200=CARTESIAN_POINT('',(4.87765050780098,-8.47904220774524,25.6171005248744));
#17201=CARTESIAN_POINT('Ctrl Pts',(4.87765050780186,-8.47904220774555,25.6171005248744));
#17202=CARTESIAN_POINT('Ctrl Pts',(4.87588972264421,-8.4838799252067,25.6174357889926));
#17203=CARTESIAN_POINT('Ctrl Pts',(4.87402473097088,-8.4886816676111,25.6177907069695));
#17204=CARTESIAN_POINT('Ctrl Pts',(4.85375038183513,-8.53774339253776,25.6216464793742));
#17205=CARTESIAN_POINT('Ctrl Pts',(4.8261873242743,-8.57811228796921,25.6268660950636));
#17206=CARTESIAN_POINT('Ctrl Pts',(4.76233566045074,-8.64238213104608,25.6388093849193));
#17207=CARTESIAN_POINT('Ctrl Pts',(4.72157397512207,-8.67035725543921,25.6463663780933));
#17208=CARTESIAN_POINT('Ctrl Pts',(4.63237064684611,-8.70741157798234,25.6626286921697));
#17209=CARTESIAN_POINT('Ctrl Pts',(4.58392896676938,-8.71649372935709,25.6713270794946));
#17210=CARTESIAN_POINT('Ctrl Pts',(4.53853459051412,-8.71649372935709,25.679350021924));
#17211=CARTESIAN_POINT('',(5.62533193759163,-6.42480436245001,25.4633649459313));
#17212=CARTESIAN_POINT('Origin',(0.,-21.8802768379213,0.));
#17213=CARTESIAN_POINT('',(5.28621602030355,-5.94049664112041,25.5359204644057));
#17214=CARTESIAN_POINT('Ctrl Pts',(5.28621602030455,-5.94049664112042,25.5359204644058));
#17215=CARTESIAN_POINT('Ctrl Pts',(5.33136843212714,-5.9404966411203,25.5265734192086));
#17216=CARTESIAN_POINT('Ctrl Pts',(5.37958162240371,-5.9494811318656,25.5164550937477));
#17217=CARTESIAN_POINT('Ctrl Pts',(5.46848287687259,-5.98621580905064,25.4975503530967));
#17218=CARTESIAN_POINT('Ctrl Pts',(5.50917071411043,-6.01397010132902,25.4887708497331));
#17219=CARTESIAN_POINT('Ctrl Pts',(5.57322358148026,-6.07802296869885,25.4748415806528));
#17220=CARTESIAN_POINT('Ctrl Pts',(5.60100462334978,-6.11845716197963,25.4687341407119));
#17221=CARTESIAN_POINT('Ctrl Pts',(5.63794408359696,-6.20736226972025,25.4605824370093));
#17222=CARTESIAN_POINT('Ctrl Pts',(5.64709564177536,-6.25583686010922,25.458547181456));
#17223=CARTESIAN_POINT('Ctrl Pts',(5.64709564177536,-6.30137626259124,25.458547181456));
#17224=CARTESIAN_POINT('Ctrl Pts',(5.64709564177536,-6.34181168129688,25.458547181456));
#17225=CARTESIAN_POINT('Ctrl Pts',(5.63995774538189,-6.38462028580801,25.4601338323748));
#17226=CARTESIAN_POINT('Ctrl Pts',(5.62533193759256,-6.42480436245034,25.4633649459313));
#17227=CARTESIAN_POINT('',(3.55589878430841,-5.94049664112042,25.8337550041322));
#17228=CARTESIAN_POINT('Origin',(0.,-5.94049664112045,0.));
#17229=CARTESIAN_POINT('Ctrl Pts',(3.21678286702069,-6.17794816273259,25.8781688255607));
#17230=CARTESIAN_POINT('Ctrl Pts',(3.21859300647374,-6.17297484545925,25.8779438163795));
#17231=CARTESIAN_POINT('Ctrl Pts',(3.22051350443719,-6.168038928994,25.8777048967159));
#17232=CARTESIAN_POINT('Ctrl Pts',(3.24097554860329,-6.11869160409763,25.8751567407837));
#17233=CARTESIAN_POINT('Ctrl Pts',(3.26875389341492,-6.07816029841708,25.8716756342651));
#17234=CARTESIAN_POINT('Ctrl Pts',(3.33285237724758,-6.01406181458443,25.8634966355504));
#17235=CARTESIAN_POINT('Ctrl Pts',(3.37350118572857,-5.9862885785338,25.8582446214298));
#17236=CARTESIAN_POINT('Ctrl Pts',(3.46242406986543,-5.94950752252592,25.8464880537427));
#17237=CARTESIAN_POINT('Ctrl Pts',(3.51069601433232,-5.94049664112043,25.8399769596623));
#17238=CARTESIAN_POINT('Ctrl Pts',(3.55589878430884,-5.94049664112043,25.8337550041323));
#17239=CARTESIAN_POINT('Origin',(2.80821735451831,-8.71649372935708,27.4319999999998));
#17240=CARTESIAN_POINT('',(4.53853459051412,-8.71649372935708,27.432));
#17241=CARTESIAN_POINT('Origin',(4.87765050780198,-8.47904220774524,27.432));
#17242=CARTESIAN_POINT('',(4.87765050780198,-8.47904220774524,27.432));
#17243=CARTESIAN_POINT('',(5.62533193759263,-6.42480436245001,27.432));
#17244=CARTESIAN_POINT('Origin',(5.28621602030455,-5.94049664112042,27.432));
#17245=CARTESIAN_POINT('',(5.28621602030455,-5.94049664112042,27.432));
#17246=CARTESIAN_POINT('',(3.55589878430884,-5.94049664112042,27.4319999999999));
#17247=CARTESIAN_POINT('Origin',(3.21678286702076,-6.17794816273248,27.4319999999996));
#17248=CARTESIAN_POINT('',(3.21678286702076,-6.17794816273248,27.4319999999996));
#17249=CARTESIAN_POINT('Origin',(4.53853459051412,-8.35561410788657,27.432));
#17250=CARTESIAN_POINT('Origin',(5.28621602030455,-6.30137626259123,27.432));
#17251=CARTESIAN_POINT('Origin',(3.55589878430884,-6.30137626259121,27.4319999999999));
#17252=CARTESIAN_POINT('Origin',(48.91024,-73.5076,-14.732));
#17253=CARTESIAN_POINT('Origin',(48.9102399999989,-5.715,14.732));
#17254=CARTESIAN_POINT('',(0.,0.,0.));
#17255=CARTESIAN_POINT('Origin',(3.556,0.,0.));
#17256=CARTESIAN_POINT('',(3.556,-4.80588143389396E-16,3.9243));
#17257=CARTESIAN_POINT('Origin',(3.556,0.,0.));
#17258=CARTESIAN_POINT('',(3.048,-5.42800200786081E-16,4.4323));
#17259=CARTESIAN_POINT('Origin',(3.556,-5.42800200786081E-16,4.4323));
#17260=CARTESIAN_POINT('Origin',(3.048,0.,0.));
#17261=CARTESIAN_POINT('Origin',(42.926,0.,0.));
#17262=CARTESIAN_POINT('',(32.7025,-4.80588143389396E-16,3.9243));
#17263=CARTESIAN_POINT('Origin',(32.7025,0.,0.));
#17264=CARTESIAN_POINT('',(42.926,-4.80588143389396E-16,3.9243));
#17265=CARTESIAN_POINT('Origin',(32.7025,0.,0.));
#17266=CARTESIAN_POINT('',(33.2105,-4.1837608599271E-16,3.4163));
#17267=CARTESIAN_POINT('Origin',(33.2105,0.,0.));
#17268=CARTESIAN_POINT('Origin',(32.7025,-4.1837608599271E-16,3.4163));
#17269=CARTESIAN_POINT('Origin',(42.926,0.,0.));
#17270=CARTESIAN_POINT('',(41.9354,3.88825358729285E-16,-3.175));
#17271=CARTESIAN_POINT('',(41.9354,-3.88825358729285E-16,3.175));
#17272=CARTESIAN_POINT('Origin',(41.9354,0.,0.));
#17273=CARTESIAN_POINT('Origin',(41.9354,0.,0.));
#17274=CARTESIAN_POINT('',(33.2105,-3.88825358729285E-16,3.175));
#17275=CARTESIAN_POINT('',(42.926,-3.88825358729285E-16,3.175));
#17276=CARTESIAN_POINT('Origin',(33.2105,0.,0.));
#17277=CARTESIAN_POINT('Origin',(41.9354,0.,0.));
#17278=CARTESIAN_POINT('',(42.926,-2.67511846805748E-16,-2.1844));
#17279=CARTESIAN_POINT('',(41.9354,-3.88825358729285E-16,-3.175));
#17280=CARTESIAN_POINT('Origin',(42.926,0.,0.));
#17281=CARTESIAN_POINT('Origin',(0.,0.,0.));
#17282=CARTESIAN_POINT('',(6.97226631718919E-16,-4.83934995634745,2.794));
#17283=CARTESIAN_POINT('',(0.2316331296214,-3.22623330423164,5.588));
#17284=CARTESIAN_POINT('Ctrl Pts',(1.60507362838917E-15,-4.83934995634745,
2.794));
#17285=CARTESIAN_POINT('Ctrl Pts',(1.58206781009085E-15,-4.09069991269487,
4.09069991269492));
#17286=CARTESIAN_POINT('Ctrl Pts',(0.231633129621414,-3.22623330423158,
5.58800000000009));
#17287=CARTESIAN_POINT('',(0.,0.,5.588));
#17288=CARTESIAN_POINT('Ctrl Pts',(0.231633129621415,-3.22623330423175,
5.588));
#17289=CARTESIAN_POINT('Ctrl Pts',(7.23804935274901E-16,-1.49730008730516,
5.588));
#17290=CARTESIAN_POINT('Ctrl Pts',(7.55328766300784E-16,0.,5.588));
#17291=CARTESIAN_POINT('Origin',(0.,0.,0.));
#17292=CARTESIAN_POINT('Origin',(0.,0.,0.));
#17293=CARTESIAN_POINT('',(0.,0.,-5.588));
#17294=CARTESIAN_POINT('',(6.97226631718919E-16,4.83934995634745,-2.794));
#17295=CARTESIAN_POINT('Origin',(0.,0.,0.));
#17296=CARTESIAN_POINT('',(-8.13431070338758E-16,-4.83934995634745,-2.79399999999999));
#17297=CARTESIAN_POINT('Origin',(0.,0.,0.));
#17298=CARTESIAN_POINT('Origin',(0.,0.,0.));
#17299=CARTESIAN_POINT('',(-8.13431070338758E-16,4.83934995634745,2.79399999999999));
#17300=CARTESIAN_POINT('Origin',(0.,0.,0.));
#17301=CARTESIAN_POINT('Origin',(0.,0.,0.));
#17302=CARTESIAN_POINT('Origin',(0.,0.,0.));
#17303=CARTESIAN_POINT('',(0.2316331296214,3.22623330423164,-5.588));
#17304=CARTESIAN_POINT('Ctrl Pts',(1.60507362838917E-15,4.83934995634745,
-2.794));
#17305=CARTESIAN_POINT('Ctrl Pts',(1.58206781009085E-15,4.09069991269487,
-4.09069991269492));
#17306=CARTESIAN_POINT('Ctrl Pts',(0.231633129621414,3.22623330423158,-5.58800000000009));
#17307=CARTESIAN_POINT('Ctrl Pts',(0.231633129621415,3.22623330423175,-5.588));
#17308=CARTESIAN_POINT('Ctrl Pts',(7.23804935274901E-16,1.49730008730516,
-5.588));
#17309=CARTESIAN_POINT('Ctrl Pts',(7.55328766300784E-16,0.,-5.588));
#17310=CARTESIAN_POINT('Origin',(0.,0.,0.));
#17311=CARTESIAN_POINT('',(0.231633129621398,-3.22623330423163,-5.588));
#17312=CARTESIAN_POINT('Ctrl Pts',(7.55328766300784E-16,0.,-5.588));
#17313=CARTESIAN_POINT('Ctrl Pts',(7.49400541621981E-16,-1.49730008730516,
-5.588));
#17314=CARTESIAN_POINT('Ctrl Pts',(0.231633129621414,-3.22623330423174,
-5.588));
#17315=CARTESIAN_POINT('Ctrl Pts',(0.23163312962141,-3.22623330423158,-5.58800000000008));
#17316=CARTESIAN_POINT('Ctrl Pts',(-3.23084588979102E-15,-4.09069991269487,
-4.09069991269491));
#17317=CARTESIAN_POINT('Ctrl Pts',(-2.26598629890234E-15,-4.83934995634745,
-2.79399999999998));
#17318=CARTESIAN_POINT('Origin',(0.,0.,0.));
#17319=CARTESIAN_POINT('',(0.231633129621398,-6.45246660846325,3.02488368589446E-15));
#17320=CARTESIAN_POINT('Ctrl Pts',(-2.26598629890234E-15,-4.83934995634745,
-2.79399999999998));
#17321=CARTESIAN_POINT('Ctrl Pts',(-1.33226762955019E-15,-5.58800000000002,
-1.49730008730506));
#17322=CARTESIAN_POINT('Ctrl Pts',(0.231633129621411,-6.45246660846331,
9.96848220883504E-14));
#17323=CARTESIAN_POINT('Ctrl Pts',(0.231633129621414,-6.45246660846331,
-8.86991478173896E-14));
#17324=CARTESIAN_POINT('Ctrl Pts',(1.66560959941808E-15,-5.58800000000003,
1.49730008730508));
#17325=CARTESIAN_POINT('Ctrl Pts',(1.60507362838917E-15,-4.83934995634745,
2.794));
#17326=CARTESIAN_POINT('Origin',(0.,0.,0.));
#17327=CARTESIAN_POINT('',(0.231633129621398,3.22623330423163,5.588));
#17328=CARTESIAN_POINT('Ctrl Pts',(7.55328766300784E-16,0.,5.588));
#17329=CARTESIAN_POINT('Ctrl Pts',(7.49400541621981E-16,1.49730008730516,
5.588));
#17330=CARTESIAN_POINT('Ctrl Pts',(0.231633129621414,3.22623330423174,5.588));
#17331=CARTESIAN_POINT('Ctrl Pts',(0.23163312962141,3.22623330423158,5.58800000000008));
#17332=CARTESIAN_POINT('Ctrl Pts',(-3.23084588979102E-15,4.09069991269487,
4.09069991269491));
#17333=CARTESIAN_POINT('Ctrl Pts',(-2.26598629890234E-15,4.83934995634745,
2.79399999999998));
#17334=CARTESIAN_POINT('Origin',(0.,0.,0.));
#17335=CARTESIAN_POINT('',(0.231633129621398,6.45246660846325,-3.02488368589446E-15));
#17336=CARTESIAN_POINT('Ctrl Pts',(-2.26598629890234E-15,4.83934995634745,
2.79399999999998));
#17337=CARTESIAN_POINT('Ctrl Pts',(-1.33226762955019E-15,5.58800000000002,
1.49730008730506));
#17338=CARTESIAN_POINT('Ctrl Pts',(0.231633129621411,6.45246660846331,-9.96848220883504E-14));
#17339=CARTESIAN_POINT('Ctrl Pts',(0.231633129621414,6.45246660846331,8.86991478173896E-14));
#17340=CARTESIAN_POINT('Ctrl Pts',(1.66560959941808E-15,5.58800000000003,
-1.49730008730508));
#17341=CARTESIAN_POINT('Ctrl Pts',(1.60507362838917E-15,4.83934995634745,
-2.794));
#17342=CARTESIAN_POINT('Origin',(3.048,-3.22623330423164,5.588));
#17343=CARTESIAN_POINT('',(3.048,-6.45246660846325,0.));
#17344=CARTESIAN_POINT('',(3.048,-6.45246660846325,0.));
#17345=CARTESIAN_POINT('',(3.048,-3.22623330423164,5.588));
#17346=CARTESIAN_POINT('',(3.048,-3.22623330423164,5.588));
#17347=CARTESIAN_POINT('',(3.048,-3.22623330423164,5.588));
#17348=CARTESIAN_POINT('Origin',(3.048,-6.45246660846325,0.));
#17349=CARTESIAN_POINT('',(3.048,-3.22623330423164,-5.588));
#17350=CARTESIAN_POINT('',(3.048,-3.22623330423164,-5.588));
#17351=CARTESIAN_POINT('',(3.048,-6.45246660846325,0.));
#17352=CARTESIAN_POINT('Origin',(3.048,-3.22623330423164,-5.588));
#17353=CARTESIAN_POINT('',(3.048,3.22623330423164,-5.588));
#17354=CARTESIAN_POINT('',(3.048,3.22623330423164,-5.588));
#17355=CARTESIAN_POINT('',(3.048,-3.22623330423164,-5.588));
#17356=CARTESIAN_POINT('Origin',(3.048,3.22623330423164,-5.588));
#17357=CARTESIAN_POINT('',(3.048,6.45246660846325,0.));
#17358=CARTESIAN_POINT('',(3.048,6.45246660846325,0.));
#17359=CARTESIAN_POINT('',(3.048,3.22623330423164,-5.588));
#17360=CARTESIAN_POINT('Origin',(3.048,6.45246660846325,0.));
#17361=CARTESIAN_POINT('',(3.048,3.22623330423164,5.588));
#17362=CARTESIAN_POINT('',(3.048,3.22623330423164,5.588));
#17363=CARTESIAN_POINT('',(3.048,6.45246660846325,0.));
#17364=CARTESIAN_POINT('Origin',(3.048,3.22623330423164,5.588));
#17365=CARTESIAN_POINT('',(3.048,3.22623330423164,5.588));
#17366=CARTESIAN_POINT('Origin',(42.926,2.1844,0.));
#17367=CARTESIAN_POINT('Origin',(33.2105,3.4163,0.));
#17368=CARTESIAN_POINT('Origin',(3.048,6.7056,0.));
#17369=CARTESIAN_POINT('',(0.,0.,0.));
#17370=CARTESIAN_POINT('Origin',(0.,-9.4742,0.));
#17371=CARTESIAN_POINT('',(-6.92109138538127E-16,-6.6802,5.6515));
#17372=CARTESIAN_POINT('Origin',(0.,-6.6802,0.));
#17373=CARTESIAN_POINT('',(-6.92109138538127E-16,-9.4742,5.6515));
#17374=CARTESIAN_POINT('',(-6.92109138538127E-16,-9.4742,5.6515));
#17375=CARTESIAN_POINT('Origin',(0.,-9.4742,0.));
#17376=CARTESIAN_POINT('Origin',(0.,-8.3312,0.));
#17377=CARTESIAN_POINT('',(-1.0436492248112E-15,-9.4742,8.52204264558423));
#17378=CARTESIAN_POINT('Origin',(0.,-9.4742,0.));
#17379=CARTESIAN_POINT('',(-1.17518470014524E-15,-8.72212902382124,9.59611131114252));
#17380=CARTESIAN_POINT('Origin',(-1.0436492248112E-15,-8.3312,8.52204264558423));
#17381=CARTESIAN_POINT('',(1.22323286863573E-15,-8.72212902382124,-9.59611131114252));
#17382=CARTESIAN_POINT('Origin',(0.,-8.72212902382124,0.));
#17383=CARTESIAN_POINT('Origin',(0.,-8.72212902382124,0.));
#17384=CARTESIAN_POINT('Origin',(0.,-8.72212902382124,0.));
#17385=CARTESIAN_POINT('',(1.65064649448932E-15,-6.72999068591485,10.3807974512434));
#17386=CARTESIAN_POINT('',(-1.27128103712622E-15,-6.72999068591485,-10.3807974512434));
#17387=CARTESIAN_POINT('Origin',(0.,-6.72999068591485,0.));
#17388=CARTESIAN_POINT('Origin',(0.,-6.72999068591485,0.));
#17389=CARTESIAN_POINT('',(-1.17518470014524E-15,-8.72212902382124,-9.59611131114252));
#17390=CARTESIAN_POINT('Origin',(0.,-3.38913168859475,0.));
#17391=CARTESIAN_POINT('',(-2.03001195185241E-15,-4.43601779450536,16.5763055377745));
#17392=CARTESIAN_POINT('Origin',(0.,-4.43601779450534,0.));
#17393=CARTESIAN_POINT('',(-2.14554140320065E-15,-5.22267163670422,17.5196750989302));
#17394=CARTESIAN_POINT('',(-1.87626430460025E-15,-3.38913168859475,15.3208607241417));
#17395=CARTESIAN_POINT('Origin',(0.,-5.22267163670421,0.));
#17396=CARTESIAN_POINT('Origin',(0.,-4.0132,0.));
#17397=CARTESIAN_POINT('',(-2.26905317419133E-15,-5.588,18.5282252464232));
#17398=CARTESIAN_POINT('Origin',(-2.26905317419134E-15,-4.0132,18.5282252464232));
#17399=CARTESIAN_POINT('Origin',(0.,-5.588,0.));
#17400=CARTESIAN_POINT('Origin',(0.,-9.4742,0.));
#17401=CARTESIAN_POINT('',(-2.33295215237571E-15,-5.588,19.05));
#17402=CARTESIAN_POINT('Origin',(0.,-5.588,0.));
#17403=CARTESIAN_POINT('',(-2.33295215237571E-15,-2.794,19.05));
#17404=CARTESIAN_POINT('',(-2.33295215237571E-15,-9.4742,19.05));
#17405=CARTESIAN_POINT('Origin',(0.,-2.794,0.));
#17406=CARTESIAN_POINT('Origin',(0.,-2.0066,0.));
#17407=CARTESIAN_POINT('',(-2.26106256679795E-15,-2.794,18.4629769854638));
#17408=CARTESIAN_POINT('Origin',(0.,-2.794,0.));
#17409=CARTESIAN_POINT('',(-2.17916487105407E-15,-2.4222660944206,17.7942315496296));
#17410=CARTESIAN_POINT('Origin',(-2.26106256679795E-15,-2.0066,18.4629769854638));
#17411=CARTESIAN_POINT('Origin',(0.,-2.4222660944206,0.));
#17412=CARTESIAN_POINT('Origin',(0.,-5.1308,0.));
#17413=CARTESIAN_POINT('',(-1.64550891814233E-15,0.,13.4366));
#17414=CARTESIAN_POINT('Origin',(-1.64550891814233E-15,-5.1308,13.4366));
#17415=CARTESIAN_POINT('Origin',(0.,0.,0.));
#17416=CARTESIAN_POINT('Origin',(0.,-5.1308,0.));
#17417=CARTESIAN_POINT('',(-1.63980436590338E-15,0.,13.3900187959915));
#17418=CARTESIAN_POINT('Origin',(0.,0.,0.));
#17419=CARTESIAN_POINT('',(-1.04935623218168E-15,-3.37596304862466,8.56864389726312));
#17420=CARTESIAN_POINT('Origin',(-1.63980436590338E-15,-5.1308,13.3900187959915));
#17421=CARTESIAN_POINT('',(1.04935623218168E-15,-3.37596304862466,-8.56864389726312));
#17422=CARTESIAN_POINT('Origin',(0.,-3.37596304862466,0.));
#17423=CARTESIAN_POINT('Origin',(0.,-3.37596304862466,0.));
#17424=CARTESIAN_POINT('Origin',(0.,-3.37596304862466,0.));
#17425=CARTESIAN_POINT('',(9.35597266583422E-16,-5.92812902382124,7.6397314493846));
#17426=CARTESIAN_POINT('',(-9.35597266583421E-16,-5.92812902382124,-7.63973144938459));
#17427=CARTESIAN_POINT('Origin',(0.,-5.92812902382124,0.));
#17428=CARTESIAN_POINT('',(-1.04935623218168E-15,-3.37596304862466,-8.56864389726312));
#17429=CARTESIAN_POINT('Origin',(0.,-5.92812902382124,0.));
#17430=CARTESIAN_POINT('Origin',(0.,-5.5372,0.));
#17431=CARTESIAN_POINT('',(-8.04061791249378E-16,-6.6802,6.5656627838263));
#17432=CARTESIAN_POINT('Origin',(-8.04061791249378E-16,-5.5372,6.5656627838263));
#17433=CARTESIAN_POINT('Origin',(0.,-6.6802,0.));
#17434=CARTESIAN_POINT('Origin',(0.,-6.1214,0.));
#17435=CARTESIAN_POINT('Origin',(-1.67505964540576E-15,-6.1214,13.6779));
#17436=CARTESIAN_POINT('Origin',(13.4366,0.,0.));
#17437=CARTESIAN_POINT('Origin',(19.05,-2.794,0.));
#17438=CARTESIAN_POINT('Origin',(18.5282252464232,-5.588,0.));
#17439=CARTESIAN_POINT('Origin',(5.6515,-9.4742,0.));
#17440=CARTESIAN_POINT('Origin',(6.5656627838263,-6.6802,0.));
#17441=CARTESIAN_POINT('',(0.,0.,0.));
#17442=CARTESIAN_POINT('Origin',(4.0132,0.,0.));
#17443=CARTESIAN_POINT('',(4.0132,-6.73445521319121E-16,5.4991));
#17444=CARTESIAN_POINT('Origin',(4.0132,0.,0.));
#17445=CARTESIAN_POINT('',(3.6068,0.,5.4991));
#17446=CARTESIAN_POINT('',(4.0132,-6.73445521319121E-16,5.4991));
#17447=CARTESIAN_POINT('',(3.6068,-4.76236029795101,2.74955));
#17448=CARTESIAN_POINT('Origin',(3.6068,0.,0.));
#17449=CARTESIAN_POINT('',(3.6068,-4.76236029795101,-2.74955));
#17450=CARTESIAN_POINT('Origin',(3.6068,0.,0.));
#17451=CARTESIAN_POINT('',(3.6068,0.,-5.4991));
#17452=CARTESIAN_POINT('Origin',(3.6068,0.,0.));
#17453=CARTESIAN_POINT('',(3.6068,4.76236029795101,-2.74955));
#17454=CARTESIAN_POINT('Origin',(3.6068,0.,0.));
#17455=CARTESIAN_POINT('',(3.6068,4.76236029795101,2.74955));
#17456=CARTESIAN_POINT('Origin',(3.6068,0.,0.));
#17457=CARTESIAN_POINT('Origin',(3.6068,0.,0.));
#17458=CARTESIAN_POINT('Origin',(0.,0.,0.));
#17459=CARTESIAN_POINT('',(0.68707,3.04683551100267E-16,2.48793));
#17460=CARTESIAN_POINT('',(0.687070000000001,-3.04683551100267E-16,-2.48793));
#17461=CARTESIAN_POINT('Origin',(0.68707,0.,0.));
#17462=CARTESIAN_POINT('',(-2.24879295770376E-16,-3.88825358729285E-16,
-3.175));
#17463=CARTESIAN_POINT('',(0.,-3.88825358729285E-16,-3.175));
#17464=CARTESIAN_POINT('Origin',(0.,0.,0.));
#17465=CARTESIAN_POINT('Origin',(0.68707,0.,0.));
#17466=CARTESIAN_POINT('Origin',(4.0132,0.,0.));
#17467=CARTESIAN_POINT('',(3.32613,-3.04683551100267E-16,2.48793));
#17468=CARTESIAN_POINT('',(4.0132,-3.04683551100267E-16,2.48793));
#17469=CARTESIAN_POINT('Origin',(3.32613,0.,0.));
#17470=CARTESIAN_POINT('Origin',(3.32613,0.,0.));
#17471=CARTESIAN_POINT('',(4.0132,-3.88825358729285E-16,3.175));
#17472=CARTESIAN_POINT('',(3.32613,-3.04683551100267E-16,2.48793));
#17473=CARTESIAN_POINT('Origin',(4.0132,0.,0.));
#17474=CARTESIAN_POINT('Origin',(0.,0.,0.));
#17475=CARTESIAN_POINT('',(-1.45255548274778E-16,-4.76236029795101,2.74955));
#17476=CARTESIAN_POINT('',(0.227948057104695,-3.17490686530067,5.4991));
#17477=CARTESIAN_POINT('Ctrl Pts',(-6.0638607167382E-16,-4.76236029795101,
2.74954999999999));
#17478=CARTESIAN_POINT('Ctrl Pts',(-9.99200722162641E-16,-4.02562059590196,
4.0256205959021));
#17479=CARTESIAN_POINT('Ctrl Pts',(0.227948057104729,-3.17490686530054,
5.49910000000022));
#17480=CARTESIAN_POINT('',(0.,0.,5.4991));
#17481=CARTESIAN_POINT('Ctrl Pts',(0.227948057104731,-3.17490686530094,
5.4991));
#17482=CARTESIAN_POINT('Ctrl Pts',(1.89523333747949E-16,-1.47347940409809,
5.4991));
#17483=CARTESIAN_POINT('Ctrl Pts',(3.46506326670755E-16,1.38602530668302E-15,
5.4991));
#17484=CARTESIAN_POINT('Origin',(0.,0.,0.));
#17485=CARTESIAN_POINT('Origin',(0.,0.,0.));
#17486=CARTESIAN_POINT('',(0.,0.,-5.4991));
#17487=CARTESIAN_POINT('',(-1.45255548274778E-16,4.76236029795101,-2.74955));
#17488=CARTESIAN_POINT('Origin',(0.,0.,0.));
#17489=CARTESIAN_POINT('',(-8.71533289648669E-17,-4.76236029795101,-2.74955));
#17490=CARTESIAN_POINT('Origin',(0.,0.,0.));
#17491=CARTESIAN_POINT('Origin',(0.,0.,0.));
#17492=CARTESIAN_POINT('',(-8.71533289648669E-17,4.76236029795101,2.74955));
#17493=CARTESIAN_POINT('Origin',(0.,0.,0.));
#17494=CARTESIAN_POINT('Origin',(0.,0.,0.));
#17495=CARTESIAN_POINT('Origin',(0.,0.,0.));
#17496=CARTESIAN_POINT('',(0.227948057104695,3.17490686530067,-5.4991));
#17497=CARTESIAN_POINT('Ctrl Pts',(-6.0638607167382E-16,4.76236029795101,
-2.74954999999999));
#17498=CARTESIAN_POINT('Ctrl Pts',(-9.99200722162641E-16,4.02562059590196,
-4.0256205959021));
#17499=CARTESIAN_POINT('Ctrl Pts',(0.227948057104729,3.17490686530054,-5.49910000000022));
#17500=CARTESIAN_POINT('Ctrl Pts',(0.227948057104731,3.17490686530094,-5.4991));
#17501=CARTESIAN_POINT('Ctrl Pts',(1.89523333747949E-16,1.47347940409809,
-5.4991));
#17502=CARTESIAN_POINT('Ctrl Pts',(3.46506326670755E-16,-1.38602530668302E-15,
-5.4991));
#17503=CARTESIAN_POINT('Origin',(0.,0.,0.));
#17504=CARTESIAN_POINT('',(0.227948057104695,-3.17490686530067,-5.4991));
#17505=CARTESIAN_POINT('Ctrl Pts',(3.46506326670755E-16,-1.38602530668302E-15,
-5.4991));
#17506=CARTESIAN_POINT('Ctrl Pts',(4.71844785465692E-16,-1.47347940409809,
-5.4991));
#17507=CARTESIAN_POINT('Ctrl Pts',(0.227948057104729,-3.17490686530093,
-5.4991));
#17508=CARTESIAN_POINT('Ctrl Pts',(0.22794805710473,-3.17490686530054,-5.49910000000023));
#17509=CARTESIAN_POINT('Ctrl Pts',(-4.36421435310789E-16,-4.02562059590196,
-4.02562059590211));
#17510=CARTESIAN_POINT('Ctrl Pts',(-6.06386071673821E-16,-4.762360297951,
-2.74955));
#17511=CARTESIAN_POINT('Origin',(0.,0.,0.));
#17512=CARTESIAN_POINT('',(0.227948057104694,-6.34981373060134,-4.28887208897701E-17));
#17513=CARTESIAN_POINT('Ctrl Pts',(-6.06386071673821E-16,-4.762360297951,
-2.74955));
#17514=CARTESIAN_POINT('Ctrl Pts',(-8.04911692853238E-16,-5.49910000000005,
-1.4734794040979));
#17515=CARTESIAN_POINT('Ctrl Pts',(0.227948057104729,-6.34981373060147,
2.26225062694678E-13));
#17516=CARTESIAN_POINT('Ctrl Pts',(0.227948057104729,-6.34981373060147,
-2.28464914800566E-13));
#17517=CARTESIAN_POINT('Ctrl Pts',(-9.3584922122824E-17,-5.49910000000005,
1.47347940409789));
#17518=CARTESIAN_POINT('Ctrl Pts',(-6.0638607167382E-16,-4.76236029795101,
2.74954999999999));
#17519=CARTESIAN_POINT('Origin',(0.,0.,0.));
#17520=CARTESIAN_POINT('',(0.227948057104695,3.17490686530067,5.4991));
#17521=CARTESIAN_POINT('Ctrl Pts',(3.46506326670755E-16,1.38602530668302E-15,
5.4991));
#17522=CARTESIAN_POINT('Ctrl Pts',(4.71844785465692E-16,1.47347940409809,
5.4991));
#17523=CARTESIAN_POINT('Ctrl Pts',(0.227948057104729,3.17490686530093,5.4991));
#17524=CARTESIAN_POINT('Ctrl Pts',(0.22794805710473,3.17490686530054,5.49910000000023));
#17525=CARTESIAN_POINT('Ctrl Pts',(-4.36421435310789E-16,4.02562059590196,
4.02562059590211));
#17526=CARTESIAN_POINT('Ctrl Pts',(-6.06386071673821E-16,4.762360297951,
2.74955));
#17527=CARTESIAN_POINT('Origin',(0.,0.,0.));
#17528=CARTESIAN_POINT('',(0.227948057104694,6.34981373060134,4.28887208897701E-17));
#17529=CARTESIAN_POINT('Ctrl Pts',(-6.06386071673821E-16,4.762360297951,
2.74955));
#17530=CARTESIAN_POINT('Ctrl Pts',(-8.04911692853238E-16,5.49910000000005,
1.4734794040979));
#17531=CARTESIAN_POINT('Ctrl Pts',(0.227948057104729,6.34981373060147,-2.26225062694678E-13));
#17532=CARTESIAN_POINT('Ctrl Pts',(0.227948057104729,6.34981373060147,2.28464914800566E-13));
#17533=CARTESIAN_POINT('Ctrl Pts',(-9.3584922122824E-17,5.49910000000005,
-1.47347940409789));
#17534=CARTESIAN_POINT('Ctrl Pts',(-6.0638607167382E-16,4.76236029795101,
-2.74954999999999));
#17535=CARTESIAN_POINT('Origin',(4.0132,-3.17490686530067,5.4991));
#17536=CARTESIAN_POINT('',(3.6068,-6.34981373060134,0.));
#17537=CARTESIAN_POINT('',(4.0132,-6.34981373060134,0.));
#17538=CARTESIAN_POINT('',(3.6068,-3.112630297951,5.60696617877061));
#17539=CARTESIAN_POINT('',(3.6068,-3.17490686530067,5.4991));
#17540=CARTESIAN_POINT('',(3.6068,-3.112630297951,5.60696617877061));
#17541=CARTESIAN_POINT('',(4.0132,-3.17490686530067,5.4991));
#17542=CARTESIAN_POINT('Origin',(4.0132,-6.34981373060134,0.));
#17543=CARTESIAN_POINT('',(3.6068,-3.17490686530067,-5.4991));
#17544=CARTESIAN_POINT('',(4.0132,-3.17490686530067,-5.4991));
#17545=CARTESIAN_POINT('',(3.6068,-3.112630297951,-5.60696617877061));
#17546=CARTESIAN_POINT('',(3.6068,-3.112630297951,-5.60696617877061));
#17547=CARTESIAN_POINT('Origin',(4.0132,-3.17490686530067,-5.4991));
#17548=CARTESIAN_POINT('',(3.6068,3.17490686530067,-5.4991));
#17549=CARTESIAN_POINT('',(4.0132,3.17490686530067,-5.4991));
#17550=CARTESIAN_POINT('',(3.6068,6.59892,-5.4991));
#17551=CARTESIAN_POINT('',(3.6068,6.59892,-5.4991));
#17552=CARTESIAN_POINT('Origin',(4.0132,3.17490686530067,-5.4991));
#17553=CARTESIAN_POINT('',(3.6068,6.34981373060134,0.));
#17554=CARTESIAN_POINT('',(4.0132,6.34981373060134,0.));
#17555=CARTESIAN_POINT('',(3.6068,6.41209029795101,0.107866178770604));
#17556=CARTESIAN_POINT('',(3.6068,6.41209029795101,0.107866178770604));
#17557=CARTESIAN_POINT('Origin',(4.0132,6.34981373060134,0.));
#17558=CARTESIAN_POINT('',(3.6068,3.17490686530067,5.4991));
#17559=CARTESIAN_POINT('',(4.0132,3.17490686530067,5.4991));
#17560=CARTESIAN_POINT('',(3.6068,6.41209029795101,-0.107866178770604));
#17561=CARTESIAN_POINT('',(3.6068,6.41209029795101,-0.107866178770604));
#17562=CARTESIAN_POINT('Origin',(4.0132,3.17490686530067,5.4991));
#17563=CARTESIAN_POINT('',(3.6068,6.59892,5.4991));
#17564=CARTESIAN_POINT('',(3.6068,6.59892,5.4991));
#17565=CARTESIAN_POINT('Origin',(4.0132,5.4991,0.));
#17566=CARTESIAN_POINT('Origin',(3.6068,6.59892,0.));
#17567=CARTESIAN_POINT('Origin',(3.6068,6.59892,0.));
#17568=CARTESIAN_POINT('Origin',(3.6068,6.59892,0.));
#17569=CARTESIAN_POINT('Origin',(3.6068,6.59892,0.));
#17570=CARTESIAN_POINT('Origin',(3.6068,6.59892,0.));
#17571=CARTESIAN_POINT('Origin',(3.6068,6.59892,0.));
#17572=CARTESIAN_POINT('',(0.,0.,0.));
#17573=CARTESIAN_POINT('Origin',(5.8674,0.,0.));
#17574=CARTESIAN_POINT('',(6.62876449118558,3.76676807019632,3.76676807019632));
#17575=CARTESIAN_POINT('',(6.604,3.6068094902476,3.6068094902476));
#17576=CARTESIAN_POINT('Origin',(5.8674,3.74476680248583,3.74476680248583));
#17577=CARTESIAN_POINT('',(6.62876449118558,-5.32701449118557,-6.52371124564198E-16));
#17578=CARTESIAN_POINT('Origin',(6.62876449118558,9.93984464071305E-18,
0.));
#17579=CARTESIAN_POINT('',(6.62876449118558,-3.76676807019632,3.76676807019632));
#17580=CARTESIAN_POINT('Origin',(6.62876449118558,9.93984464071305E-18,
0.));
#17581=CARTESIAN_POINT('',(6.604,-3.6068094902476,3.6068094902476));
#17582=CARTESIAN_POINT('Origin',(5.8674,-3.74476680248583,3.74476680248583));
#17583=CARTESIAN_POINT('Origin',(6.604,9.61653668789852E-18,0.));
#17584=CARTESIAN_POINT('Origin',(6.604,8.62172254777109E-17,0.));
#17585=CARTESIAN_POINT('',(6.858,-5.55625,-6.80444377776248E-16));
#17586=CARTESIAN_POINT('Origin',(6.858,8.9533272611469E-17,0.));
#17587=CARTESIAN_POINT('',(6.604,-5.30225,-6.49338349077905E-16));
#17588=CARTESIAN_POINT('',(6.604,3.74925693054637,3.74925693054637));
#17589=CARTESIAN_POINT('',(1.30174999999991,3.23653424897184E-16,-3.06658683336675E-16));
#17590=CARTESIAN_POINT('',(6.604,-3.74925693054637,3.74925693054637));
#17591=CARTESIAN_POINT('Origin',(6.604,8.62172254777109E-17,0.));
#17592=CARTESIAN_POINT('',(1.30174999999991,1.69947415605091E-17,0.));
#17593=CARTESIAN_POINT('Origin',(0.,0.,0.));
#17594=CARTESIAN_POINT('',(1.524,-5.55625,-6.80444377776248E-16));
#17595=CARTESIAN_POINT('Origin',(1.524,1.98962828025486E-17,0.));
#17596=CARTESIAN_POINT('',(-1.58418895642851E-17,-4.03225,-4.93808205586192E-16));
#17597=CARTESIAN_POINT('',(5.26422482484099E-17,-4.03225,-4.93808205586192E-16));
#17598=CARTESIAN_POINT('Origin',(0.,0.,0.));
#17599=CARTESIAN_POINT('Origin',(54.0004,7.04991620636974E-16,0.));
#17600=CARTESIAN_POINT('',(3.048,-5.55625,-6.80444377776248E-16));
#17601=CARTESIAN_POINT('Origin',(3.048,3.97925656050972E-17,0.));
#17602=CARTESIAN_POINT('',(54.0004,-5.55625,-6.80444377776248E-16));
#17603=CARTESIAN_POINT('Origin',(3.3655,0.,0.));
#17604=CARTESIAN_POINT('',(3.3655,-3.5687,-4.37039703211716E-16));
#17605=CARTESIAN_POINT('Origin',(3.3655,4.3937624522295E-17,0.));
#17606=CARTESIAN_POINT('',(3.048,-3.8862,-4.75922239084644E-16));
#17607=CARTESIAN_POINT('Origin',(3.3655,-3.8862,-4.75922239084644E-16));
#17608=CARTESIAN_POINT('Origin',(3.048,3.97925656050972E-17,0.));
#17609=CARTESIAN_POINT('Origin',(54.0004,7.04991620636974E-16,0.));
#17610=CARTESIAN_POINT('',(6.604,-3.5687,-4.37039703211716E-16));
#17611=CARTESIAN_POINT('Origin',(6.604,8.62172254777109E-17,0.));
#17612=CARTESIAN_POINT('',(54.0004,-3.5687,-4.37039703211716E-16));
#17613=CARTESIAN_POINT('Origin',(54.0004,7.04991620636974E-16,0.));
#17614=CARTESIAN_POINT('',(37.592,-5.55625,-6.80444377776248E-16));
#17615=CARTESIAN_POINT('Origin',(37.592,4.90774975796201E-16,0.));
#17616=CARTESIAN_POINT('',(54.0004,-5.55625,-6.80444377776248E-16));
#17617=CARTESIAN_POINT('Origin',(37.592,8.67361737988404E-16,0.));
#17618=CARTESIAN_POINT('',(38.1,-6.06425,-7.42656435172934E-16));
#17619=CARTESIAN_POINT('Origin',(38.1,4.97407070063718E-16,0.));
#17620=CARTESIAN_POINT('Origin',(37.592,-6.06425,-7.42656435172934E-16));
#17621=CARTESIAN_POINT('Origin',(54.0004,7.04991620636974E-16,0.));
#17622=CARTESIAN_POINT('',(44.0309,9.525,1.16647607618785E-15));
#17623=CARTESIAN_POINT('',(44.0309,-9.525,-1.16647607618785E-15));
#17624=CARTESIAN_POINT('Origin',(44.0309,5.74836770636969E-16,0.));
#17625=CARTESIAN_POINT('Origin',(44.0309,5.74836770636969E-16,0.));
#17626=CARTESIAN_POINT('',(38.1,-9.525,-1.16647607618785E-15));
#17627=CARTESIAN_POINT('',(54.0004,-9.525,-1.16647607618785E-15));
#17628=CARTESIAN_POINT('Origin',(38.1,4.97407070063718E-16,0.));
#17629=CARTESIAN_POINT('Origin',(44.0309,5.74836770636969E-16,0.));
#17630=CARTESIAN_POINT('',(44.8564,8.6995,-1.06538148291824E-15));
#17631=CARTESIAN_POINT('',(44.0309,9.525,-1.16647607618785E-15));
#17632=CARTESIAN_POINT('Origin',(44.8564,5.85613923821682E-16,0.));
#17633=CARTESIAN_POINT('Origin',(45.3644,8.67361737988404E-16,0.));
#17634=CARTESIAN_POINT('',(45.3644,-5.4991,-6.73445521319121E-16));
#17635=CARTESIAN_POINT('Origin',(45.3644,5.92246018089199E-16,0.));
#17636=CARTESIAN_POINT('',(44.8564,-6.0071,-7.35657578715807E-16));
#17637=CARTESIAN_POINT('Origin',(45.3644,-6.0071,-7.35657578715806E-16));
#17638=CARTESIAN_POINT('Origin',(44.8564,5.85613923821682E-16,0.));
#17639=CARTESIAN_POINT('Origin',(54.0004,7.04991620636974E-16,0.));
#17640=CARTESIAN_POINT('',(51.4604,-5.4991,-6.73445521319121E-16));
#17641=CARTESIAN_POINT('Origin',(51.4604,6.71831149299393E-16,0.));
#17642=CARTESIAN_POINT('',(54.0004,-5.4991,-6.73445521319121E-16));
#17643=CARTESIAN_POINT('Origin',(51.4604,6.71831149299393E-16,0.));
#17644=CARTESIAN_POINT('',(54.0004,-8.6995,-1.06538148291824E-15));
#17645=CARTESIAN_POINT('Origin',(54.0004,7.04991620636974E-16,0.));
#17646=CARTESIAN_POINT('',(51.4604,-5.4991,-6.73445521319121E-16));
#17647=CARTESIAN_POINT('Origin',(5.8674,3.74476680248583,3.74476680248583));
#17648=CARTESIAN_POINT('',(6.604,1.78435,1.78435));
#17649=CARTESIAN_POINT('Origin',(5.8674,-3.74476680248583,3.74476680248583));
#17650=CARTESIAN_POINT('',(6.604,1.78435,-1.78435));
#17651=CARTESIAN_POINT('Origin',(54.0004,8.6995,0.));
#17652=CARTESIAN_POINT('Origin',(44.8564,8.6995,0.));
#17653=CARTESIAN_POINT('Origin',(38.1,6.06425,0.));
#17654=CARTESIAN_POINT('Origin',(3.048,5.55625,0.));
#17655=CARTESIAN_POINT('Origin',(2.6321124124205E-17,3.43630268540794E-34,
0.));
#17656=CARTESIAN_POINT('Origin',(6.604,3.5687,0.));
#17657=CARTESIAN_POINT('',(0.,0.,0.));
#17658=CARTESIAN_POINT('Origin',(0.,4.394073,0.));
#17659=CARTESIAN_POINT('',(-1.96328272378357E-15,6.72324585925114,16.0314200400514));
#17660=CARTESIAN_POINT('Origin',(0.,6.72324585925114,0.));
#17661=CARTESIAN_POINT('',(-2.117828241439E-15,6.72324585925114,17.2933799599486));
#17662=CARTESIAN_POINT('Origin',(-2.04055548261129E-15,4.394073,16.6624));
#17663=CARTESIAN_POINT('Origin',(0.,6.72324585925114,0.));
#17664=CARTESIAN_POINT('Origin',(0.,3.3528,0.));
#17665=CARTESIAN_POINT('',(1.72214462047976E-15,5.58840430174598,-14.0623779989364));
#17666=CARTESIAN_POINT('',(-1.72214462047976E-15,5.58840430174598,14.0623779989364));
#17667=CARTESIAN_POINT('Origin',(0.,5.58840430174598,0.));
#17668=CARTESIAN_POINT('Origin',(0.,5.58840430174598,0.));
#17669=CARTESIAN_POINT('Origin',(-2.04055548261129E-15,3.3528,16.6624));
#17670=CARTESIAN_POINT('Origin',(0.,0.,0.));
#17671=CARTESIAN_POINT('',(-6.9055383710321E-16,3.048,5.6388));
#17672=CARTESIAN_POINT('Origin',(0.,3.048,0.));
#17673=CARTESIAN_POINT('',(-6.9055383710321E-16,0.,5.6388));
#17674=CARTESIAN_POINT('',(-6.9055383710321E-16,0.,5.6388));
#17675=CARTESIAN_POINT('Origin',(0.,0.,0.));
#17676=CARTESIAN_POINT('Origin',(0.,0.800099999999998,0.));
#17677=CARTESIAN_POINT('',(-1.088711004442E-15,0.,8.89));
#17678=CARTESIAN_POINT('Origin',(0.,0.,0.));
#17679=CARTESIAN_POINT('',(-1.16300687227269E-15,0.278458996259272,9.49667180024818));
#17680=CARTESIAN_POINT('Origin',(-1.088711004442E-15,0.800099999999998,
8.89));
#17681=CARTESIAN_POINT('',(1.44257574637622E-15,0.278458996259272,-9.49667180024818));
#17682=CARTESIAN_POINT('Origin',(0.,0.278458996259272,0.));
#17683=CARTESIAN_POINT('Origin',(0.,0.278458996259272,0.));
#17684=CARTESIAN_POINT('Origin',(0.,0.278458996259272,0.));
#17685=CARTESIAN_POINT('',(-1.16300687227269E-15,0.278458996259272,-9.49667180024818));
#17686=CARTESIAN_POINT('Origin',(0.,3.3528,0.));
#17687=CARTESIAN_POINT('',(-2.39204713411719E-15,5.22904528301887,19.5325471456964));
#17688=CARTESIAN_POINT('Origin',(-2.04055548261129E-15,3.3528,16.6624));
#17689=CARTESIAN_POINT('Origin',(0.,5.22904528301887,0.));
#17690=CARTESIAN_POINT('Origin',(0.,7.0358,0.));
#17691=CARTESIAN_POINT('',(-2.73052057630807E-15,3.7338,22.296392545256));
#17692=CARTESIAN_POINT('Origin',(-2.73052057630807E-15,7.0358,22.296392545256));
#17693=CARTESIAN_POINT('Origin',(0.,3.7338,0.));
#17694=CARTESIAN_POINT('Origin',(0.,10.0838,0.));
#17695=CARTESIAN_POINT('',(-2.82909331011428E-15,6.84740300159127,23.1013));
#17696=CARTESIAN_POINT('Origin',(0.,6.84740300159127,0.));
#17697=CARTESIAN_POINT('',(-2.61595742103085E-15,7.81099480519482,21.3609133903113));
#17698=CARTESIAN_POINT('Origin',(-2.90929958571533E-15,10.0838,23.7562339422346));
#17699=CARTESIAN_POINT('Origin',(0.,7.81099480519482,0.));
#17700=CARTESIAN_POINT('Origin',(0.,3.3528,0.));
#17701=CARTESIAN_POINT('',(-1.35293142791519E-15,6.58152897047418,11.0475234888716));
#17702=CARTESIAN_POINT('Origin',(-2.04055548261129E-15,3.3528,16.6624));
#17703=CARTESIAN_POINT('',(1.35293142791519E-15,6.58152897047418,-11.0475234888716));
#17704=CARTESIAN_POINT('Origin',(0.,6.58152897047418,0.));
#17705=CARTESIAN_POINT('Origin',(0.,6.58152897047418,0.));
#17706=CARTESIAN_POINT('Origin',(0.,6.58152897047418,0.));
#17707=CARTESIAN_POINT('',(1.16061060402596E-15,3.85051401905933,9.4771047851023));
#17708=CARTESIAN_POINT('',(-1.16061060402596E-15,3.85051401905934,-9.47710478510228));
#17709=CARTESIAN_POINT('Origin',(0.,3.85051401905933,0.));
#17710=CARTESIAN_POINT('',(-1.35293142791519E-15,6.58152897047418,-11.0475234888716));
#17711=CARTESIAN_POINT('Origin',(0.,3.85051401905933,0.));
#17712=CARTESIAN_POINT('Origin',(0.,4.6482,0.));
#17713=CARTESIAN_POINT('',(-9.90727014042217E-16,3.048,8.0899));
#17714=CARTESIAN_POINT('Origin',(-9.90727014042217E-16,4.6482,8.0899));
#17715=CARTESIAN_POINT('Origin',(0.,3.048,0.));
#17716=CARTESIAN_POINT('Origin',(-25.019,25.4,-1.94289029309402E-13));
#17717=CARTESIAN_POINT('',(-25.019,3.7338,-1.94289029309402E-13));
#17718=CARTESIAN_POINT('',(-17.6911045585062,3.7338,17.6911045585061));
#17719=CARTESIAN_POINT('',(-18.089821188999,3.7338,16.7285174616265));
#17720=CARTESIAN_POINT('',(-17.6911045585062,6.84740300159127,17.6911045585061));
#17721=CARTESIAN_POINT('',(-17.6911045585062,25.4,17.6911045585061));
#17722=CARTESIAN_POINT('',(-25.019,6.84740300159127,-1.94289029309402E-13));
#17723=CARTESIAN_POINT('',(-17.2930919634606,6.84740300159127,18.6519919634603));
#17724=CARTESIAN_POINT('',(-25.019,25.4,-1.94289029309402E-13));
#17725=CARTESIAN_POINT('Origin',(-17.6911045585062,25.4,17.6911045585061));
#17726=CARTESIAN_POINT('',(-1.11022302462516E-12,3.7338,25.019));
#17727=CARTESIAN_POINT('',(10.1856091757486,3.7338,29.2380174616269));
#17728=CARTESIAN_POINT('',(-1.11022302462516E-12,6.84740300159127,25.019));
#17729=CARTESIAN_POINT('',(-1.11022302462516E-12,25.4,25.019));
#17730=CARTESIAN_POINT('',(14.8292874049544,6.84740300159127,31.1614919634607));
#17731=CARTESIAN_POINT('Origin',(-1.11022302462516E-12,25.4,25.019));
#17732=CARTESIAN_POINT('',(17.6911045585062,3.7338,17.691104558506));
#17733=CARTESIAN_POINT('',(27.8767137342539,3.7338,13.4720870968792));
#17734=CARTESIAN_POINT('',(17.6911045585062,6.84740300159127,17.691104558506));
#17735=CARTESIAN_POINT('',(17.6911045585062,25.4,17.691104558506));
#17736=CARTESIAN_POINT('',(32.5203919634596,6.84740300159127,11.5486125950456));
#17737=CARTESIAN_POINT('Origin',(17.6911045585062,25.4,17.691104558506));
#17738=CARTESIAN_POINT('',(25.019,3.7338,-1.11022302462516E-13));
#17739=CARTESIAN_POINT('',(24.6202833695062,3.7338,0.962587096878853));
#17740=CARTESIAN_POINT('',(25.019,6.84740300159127,-1.11022302462516E-13));
#17741=CARTESIAN_POINT('',(25.019,25.4,-1.11022302462516E-13));
#17742=CARTESIAN_POINT('',(25.4170125950456,6.84740300159127,-0.960887404954397));
#17743=CARTESIAN_POINT('Origin',(25.019,25.4,-1.11022302462516E-13));
#17744=CARTESIAN_POINT('',(17.6911045585053,3.7338,-17.6911045585064));
#17745=CARTESIAN_POINT('',(24.6202833695073,3.7338,-0.962587096879686));
#17746=CARTESIAN_POINT('',(17.6911045585053,6.84740300159127,-17.6911045585064));
#17747=CARTESIAN_POINT('',(17.6911045585053,25.4,-17.6911045585064));
#17748=CARTESIAN_POINT('',(25.4170125950445,6.84740300159127,0.960887404954397));
#17749=CARTESIAN_POINT('Origin',(17.6911045585053,25.4,-17.6911045585064));
#17750=CARTESIAN_POINT('',(0.,3.7338,-25.019));
#17751=CARTESIAN_POINT('',(27.876713734255,3.7338,-13.4720870968792));
#17752=CARTESIAN_POINT('',(0.,6.84740300159127,-25.019));
#17753=CARTESIAN_POINT('',(0.,25.4,-25.019));
#17754=CARTESIAN_POINT('',(32.5203919634607,6.84740300159127,-11.5486125950456));
#17755=CARTESIAN_POINT('Origin',(0.,25.4,-25.019));
#17756=CARTESIAN_POINT('',(-17.6911045585071,3.7338,-17.6911045585063));
#17757=CARTESIAN_POINT('',(10.1856091757476,3.7338,-29.2380174616269));
#17758=CARTESIAN_POINT('',(-17.6911045585071,6.84740300159127,-17.6911045585063));
#17759=CARTESIAN_POINT('',(-17.6911045585071,25.4,-17.6911045585063));
#17760=CARTESIAN_POINT('',(14.8292874049533,6.84740300159127,-31.1614919634607));
#17761=CARTESIAN_POINT('Origin',(-17.6911045585071,25.4,-17.6911045585063));
#17762=CARTESIAN_POINT('',(-18.089821189,3.7338,-16.7285174616273));
#17763=CARTESIAN_POINT('',(-17.2930919634617,6.84740300159127,-18.651991963461));
#17764=CARTESIAN_POINT('Origin',(27.7368,6.84740300159127,0.));
#17765=CARTESIAN_POINT('Origin',(22.2963925452559,3.7338,0.));
#17766=CARTESIAN_POINT('Origin',(5.63880000000005,0.,0.));
#17767=CARTESIAN_POINT('Origin',(8.08989999999998,3.048,-6.66133814775094E-13));
#17768=CARTESIAN_POINT('',(0.,0.,0.));
#17769=CARTESIAN_POINT('Origin',(0.,0.,13.096875));
#17770=CARTESIAN_POINT('',(14.1695751798421,-1.73527248892714E-15,4.7625));
#17771=CARTESIAN_POINT('Origin',(6.93889390390723E-15,0.,4.7625));
#17772=CARTESIAN_POINT('',(12.7,-1.55530143491714E-15,13.096875));
#17773=CARTESIAN_POINT('',(12.7,-1.55530143491714E-15,13.096875));
#17774=CARTESIAN_POINT('Origin',(0.,0.,13.096875));
#17775=CARTESIAN_POINT('Origin',(6.93889390390723E-15,0.,4.7625));
#17776=CARTESIAN_POINT('',(-36.9094469866104,-4.52010361104513E-15,4.7625));
#17777=CARTESIAN_POINT('Origin',(6.93889390390723E-15,0.,4.7625));
#17778=CARTESIAN_POINT('',(-37.465,-4.58813923300556E-15,11.1125));
#17779=CARTESIAN_POINT('',(-36.9094469866104,-4.52010361104513E-15,4.7625));
#17780=CARTESIAN_POINT('Origin',(0.,0.,11.1125));
#17781=CARTESIAN_POINT('Origin',(-1.10328413072125E-12,0.,-13.096875));
#17782=CARTESIAN_POINT('',(39.7509999999989,-4.86809349129064E-15,6.35000000000002));
#17783=CARTESIAN_POINT('Origin',(-1.11022302462516E-12,0.,6.35000000000002));
#17784=CARTESIAN_POINT('',(39.7509999999989,-4.86809349129064E-15,11.1125));
#17785=CARTESIAN_POINT('',(39.7509999999989,-4.86809349129064E-15,-13.096875));
#17786=CARTESIAN_POINT('Origin',(0.,0.,11.1125));
#17787=CARTESIAN_POINT('Origin',(0.,0.,3.048));
#17788=CARTESIAN_POINT('',(45.30725,-5.54853786906689E-15,3.048));
#17789=CARTESIAN_POINT('Origin',(0.,0.,3.048));
#17790=CARTESIAN_POINT('',(42.0052499999989,-5.1441594959883E-15,6.35000000000002));
#17791=CARTESIAN_POINT('Origin',(42.00525,-5.14415949598844E-15,3.048));
#17792=CARTESIAN_POINT('Origin',(-1.11022302462516E-12,0.,6.35000000000002));
#17793=CARTESIAN_POINT('Origin',(-1.10328413072125E-12,0.,-13.096875));
#17794=CARTESIAN_POINT('',(45.3072499999989,-5.54853786906689E-15,-3.048));
#17795=CARTESIAN_POINT('Origin',(-1.10328413072125E-12,0.,-3.048));
#17796=CARTESIAN_POINT('',(45.3072499999989,-5.54853786906689E-15,-13.096875));
#17797=CARTESIAN_POINT('Origin',(-1.10328413072125E-12,0.,-3.048));
#17798=CARTESIAN_POINT('',(42.00525,-5.14415949598857E-15,-6.35000000000002));
#17799=CARTESIAN_POINT('Origin',(6.93889390390723E-15,0.,-6.35000000000002));
#17800=CARTESIAN_POINT('Origin',(42.0052499999989,-5.14415949598844E-15,
-3.048));
#17801=CARTESIAN_POINT('Origin',(-1.10328413072125E-12,0.,-13.096875));
#17802=CARTESIAN_POINT('',(39.7509999999989,-4.86809349129064E-15,-11.1125));
#17803=CARTESIAN_POINT('Origin',(-1.10328413072125E-12,0.,-11.1125));
#17804=CARTESIAN_POINT('',(39.7509999999989,-4.86809349129064E-15,-6.35000000000002));
#17805=CARTESIAN_POINT('',(39.7509999999989,-4.86809349129064E-15,-13.096875));
#17806=CARTESIAN_POINT('Origin',(6.93889390390723E-15,0.,-6.35000000000002));
#17807=CARTESIAN_POINT('Origin',(-1.10328413072125E-12,0.,-11.1125));
#17808=CARTESIAN_POINT('',(36.9094469866093,-4.52010361104513E-15,-4.7625));
#17809=CARTESIAN_POINT('Origin',(-1.11022302462516E-12,0.,-4.7625));
#17810=CARTESIAN_POINT('',(37.4649999999989,-4.58813923300556E-15,-11.1125));
#17811=CARTESIAN_POINT('',(37.4649999999989,-4.58813923300556E-15,-11.1125));
#17812=CARTESIAN_POINT('Origin',(-1.10328413072125E-12,0.,-11.1125));
#17813=CARTESIAN_POINT('Origin',(-1.11022302462516E-12,0.,-4.7625));
#17814=CARTESIAN_POINT('',(-14.1695751798432,-1.73527248892714E-15,-4.7625));
#17815=CARTESIAN_POINT('Origin',(-1.11022302462516E-12,0.,-4.7625));
#17816=CARTESIAN_POINT('',(-12.7000000000011,-1.55530143491714E-15,-13.096875));
#17817=CARTESIAN_POINT('',(-14.1695751798432,-1.73527248892714E-15,-4.7625));
#17818=CARTESIAN_POINT('Origin',(-1.10328413072125E-12,0.,-13.096875));
#17819=CARTESIAN_POINT('Origin',(-1.10328413072125E-12,0.,-13.096875));
#17820=CARTESIAN_POINT('',(7.7215999999989,-9.4562327242962E-16,13.096875));
#17821=CARTESIAN_POINT('Origin',(0.,0.,13.096875));
#17822=CARTESIAN_POINT('',(7.7215999999989,-9.4562327242962E-16,-13.096875));
#17823=CARTESIAN_POINT('',(7.7215999999989,-9.4562327242962E-16,-13.096875));
#17824=CARTESIAN_POINT('Origin',(-1.10328413072125E-12,0.,-13.096875));
#17825=CARTESIAN_POINT('Origin',(-1.10328413072125E-12,12.7,-13.096875));
#17826=CARTESIAN_POINT('Origin',(-1.11022302462516E-12,36.9094469866104,
-4.7625));
#17827=CARTESIAN_POINT('Origin',(-1.10328413072125E-12,39.751,-11.1125));
#17828=CARTESIAN_POINT('Origin',(6.93889390390723E-15,42.00525,-6.35000000000002));
#17829=CARTESIAN_POINT('Origin',(-1.11022302462516E-12,39.751,6.35000000000002));
#17830=CARTESIAN_POINT('Origin',(0.,37.465,11.1125));
#17831=CARTESIAN_POINT('Origin',(6.93889390390723E-15,14.1695751798421,
4.7625));
#17832=CARTESIAN_POINT('Origin',(0.,0.,13.096875));
#17833=CARTESIAN_POINT('',(0.,0.,0.));
#17834=CARTESIAN_POINT('Origin',(-1.11022302462516E-12,0.,-11.1125));
#17835=CARTESIAN_POINT('',(39.7509999999989,-4.86809349129064E-15,11.1125));
#17836=CARTESIAN_POINT('Origin',(0.,0.,11.1125));
#17837=CARTESIAN_POINT('',(39.7509999999989,-4.86809349129064E-15,6.35000000000002));
#17838=CARTESIAN_POINT('',(39.7509999999989,-4.86809349129064E-15,-11.1125));
#17839=CARTESIAN_POINT('Origin',(-1.11022302462516E-12,0.,6.35000000000002));
#17840=CARTESIAN_POINT('Origin',(0.,0.,3.048));
#17841=CARTESIAN_POINT('',(42.0052499999989,-5.1441594959883E-15,6.35000000000002));
#17842=CARTESIAN_POINT('Origin',(-1.11022302462516E-12,0.,6.35000000000002));
#17843=CARTESIAN_POINT('',(45.30725,-5.54853786906689E-15,3.048));
#17844=CARTESIAN_POINT('Origin',(42.00525,-5.14415949598844E-15,3.048));
#17845=CARTESIAN_POINT('Origin',(0.,0.,3.048));
#17846=CARTESIAN_POINT('Origin',(-1.11022302462516E-12,0.,-11.1125));
#17847=CARTESIAN_POINT('',(45.3072499999989,-5.54853786906689E-15,-3.048));
#17848=CARTESIAN_POINT('',(45.3072499999989,-5.54853786906689E-15,-11.1125));
#17849=CARTESIAN_POINT('Origin',(-1.11022302462516E-12,0.,-3.048));
#17850=CARTESIAN_POINT('Origin',(-1.11022302462516E-12,0.,-3.048));
#17851=CARTESIAN_POINT('',(42.00525,-5.14415949598857E-15,-6.35000000000002));
#17852=CARTESIAN_POINT('Origin',(42.0052499999989,-5.14415949598844E-15,
-3.048));
#17853=CARTESIAN_POINT('Origin',(0.,0.,-6.35000000000002));
#17854=CARTESIAN_POINT('Origin',(-1.11022302462516E-12,0.,-11.1125));
#17855=CARTESIAN_POINT('',(39.7509999999989,-4.86809349129064E-15,-6.35000000000002));
#17856=CARTESIAN_POINT('Origin',(0.,0.,-6.35000000000002));
#17857=CARTESIAN_POINT('',(39.7509999999989,-4.86809349129064E-15,-11.1125));
#17858=CARTESIAN_POINT('',(39.7509999999989,-4.86809349129064E-15,-11.1125));
#17859=CARTESIAN_POINT('Origin',(-1.11022302462516E-12,0.,-11.1125));
#17860=CARTESIAN_POINT('Origin',(-1.11022302462516E-12,0.,-11.1125));
#17861=CARTESIAN_POINT('',(41.2749999999989,-5.0547296634807E-15,-11.1125));
#17862=CARTESIAN_POINT('Origin',(-1.11022302462516E-12,0.,-11.1125));
#17863=CARTESIAN_POINT('',(42.8625,-5.24914234284548E-15,-9.52500000000001));
#17864=CARTESIAN_POINT('Origin',(42.8624999999989,-5.24914234284534E-15,
-11.1125));
#17865=CARTESIAN_POINT('',(-42.8625,5.62252716572953E-15,-9.52500000000001));
#17866=CARTESIAN_POINT('Origin',(0.,0.,-9.52500000000001));
#17867=CARTESIAN_POINT('Origin',(0.,0.,-9.52500000000001));
#17868=CARTESIAN_POINT('Origin',(0.,0.,-9.52500000000001));
#17869=CARTESIAN_POINT('',(48.9603369133721,6.08451301965107E-15,-8.99150839805002));
#17870=CARTESIAN_POINT('',(-48.9603369133721,-5.99591198861371E-15,-8.99150839805003));
#17871=CARTESIAN_POINT('Origin',(0.,0.,-8.99150839805002));
#17872=CARTESIAN_POINT('',(-42.8625,-5.24914234284534E-15,-9.52500000000001));
#17873=CARTESIAN_POINT('Origin',(0.,0.,-8.99150839805002));
#17874=CARTESIAN_POINT('Origin',(0.,0.,-7.41004931482936));
#17875=CARTESIAN_POINT('',(50.4073015581831,-6.17311405068843E-15,-7.49313264536505));
#17876=CARTESIAN_POINT('Origin',(48.8219771717602,-5.97896780714413E-15,
-7.41004931482936));
#17877=CARTESIAN_POINT('',(-50.4073015581831,6.19715989517849E-15,-7.49313264536505));
#17878=CARTESIAN_POINT('Origin',(0.,0.,-7.49313264536505));
#17879=CARTESIAN_POINT('Origin',(0.,0.,-7.49313264536505));
#17880=CARTESIAN_POINT('Origin',(0.,0.,-7.49313264536505));
#17881=CARTESIAN_POINT('',(50.8,6.22120573966855E-15,0.));
#17882=CARTESIAN_POINT('',(-50.7999999999999,-6.22120573966855E-15,2.22044604925031E-15));
#17883=CARTESIAN_POINT('Origin',(0.,0.,0.));
#17884=CARTESIAN_POINT('',(-50.4073015581831,-6.17311405068843E-15,-7.49313264536505));
#17885=CARTESIAN_POINT('Origin',(0.,0.,0.));
#17886=CARTESIAN_POINT('Origin',(0.,0.,0.));
#17887=CARTESIAN_POINT('',(50.4073015581832,-6.17311405068844E-15,7.49313264536512));
#17888=CARTESIAN_POINT('',(50.8,-6.22120573966855E-15,0.));
#17889=CARTESIAN_POINT('Origin',(-1.11022302462516E-12,0.,7.49313264536505));
#17890=CARTESIAN_POINT('Origin',(-1.11022302462516E-12,0.,7.41004931482936));
#17891=CARTESIAN_POINT('',(48.960336913371,-5.99591198861371E-15,8.99150839805002));
#17892=CARTESIAN_POINT('Origin',(48.8219771717591,-5.97896780714413E-15,
7.41004931482936));
#17893=CARTESIAN_POINT('Origin',(-1.11022302462516E-12,0.,8.99150839805002));
#17894=CARTESIAN_POINT('Origin',(-1.11022302462516E-12,0.,8.99150839805002));
#17895=CARTESIAN_POINT('',(42.8624999999989,-5.24914234284534E-15,9.52499999999999));
#17896=CARTESIAN_POINT('',(48.960336913371,-5.99591198861371E-15,8.99150839805002));
#17897=CARTESIAN_POINT('Origin',(-1.11022302462516E-12,0.,9.52500000000001));
#17898=CARTESIAN_POINT('Origin',(0.,0.,11.1125));
#17899=CARTESIAN_POINT('',(41.275,-5.0547296634807E-15,11.1125));
#17900=CARTESIAN_POINT('Origin',(42.8625,-5.24914234284534E-15,11.1125));
#17901=CARTESIAN_POINT('Origin',(0.,0.,11.1125));
#17902=CARTESIAN_POINT('Origin',(-1.11022302462516E-12,39.751,-11.1125));
#17903=CARTESIAN_POINT('Origin',(0.,42.00525,-6.35000000000002));
#17904=CARTESIAN_POINT('Origin',(-1.11022302462516E-12,39.751,6.35000000000002));
#17905=CARTESIAN_POINT('Origin',(0.,41.275,11.1125));
#17906=CARTESIAN_POINT('',(0.,0.,0.));
#17907=CARTESIAN_POINT('Origin',(0.,0.,-14.08938));
#17908=CARTESIAN_POINT('',(4.0386,-4.9458585630365E-16,14.08938));
#17909=CARTESIAN_POINT('Origin',(0.,0.,14.08938));
#17910=CARTESIAN_POINT('',(4.0386,-4.9458585630365E-16,-14.08938));
#17911=CARTESIAN_POINT('',(4.0386,-4.9458585630365E-16,-14.08938));
#17912=CARTESIAN_POINT('Origin',(0.,0.,-14.08938));
#17913=CARTESIAN_POINT('Origin',(0.,0.,-14.08938));
#17914=CARTESIAN_POINT('',(5.55625,-6.80444377776248E-16,-14.08938));
#17915=CARTESIAN_POINT('Origin',(0.,0.,-14.08938));
#17916=CARTESIAN_POINT('',(5.55625,-6.80444377776248E-16,14.08938));
#17917=CARTESIAN_POINT('',(5.55625,-6.80444377776248E-16,-14.08938));
#17918=CARTESIAN_POINT('Origin',(0.,0.,14.08938));
#17919=CARTESIAN_POINT('Origin',(0.,4.0386,-14.08938));
#17920=CARTESIAN_POINT('Origin',(0.,5.55625,14.08938));
#17921=CARTESIAN_POINT('',(0.,0.,0.));
#17922=CARTESIAN_POINT('Origin',(0.,0.,13.09624));
#17923=CARTESIAN_POINT('',(5.6515,6.92109138538127E-16,12.71524));
#17924=CARTESIAN_POINT('',(-5.6515,-6.92109138538127E-16,12.71524));
#17925=CARTESIAN_POINT('Origin',(0.,0.,12.71524));
#17926=CARTESIAN_POINT('',(-6.0325,-7.38768181585641E-16,13.09624));
#17927=CARTESIAN_POINT('',(-6.0325,-7.38768181585641E-16,13.09624));
#17928=CARTESIAN_POINT('Origin',(0.,0.,13.09624));
#17929=CARTESIAN_POINT('Origin',(0.,0.,12.71524));
#17930=CARTESIAN_POINT('Origin',(0.,0.,-13.09624));
#17931=CARTESIAN_POINT('',(5.6515,-6.92109138538127E-16,-12.71524));
#17932=CARTESIAN_POINT('',(5.6515,-6.92109138538127E-16,-13.09624));
#17933=CARTESIAN_POINT('Origin',(0.,0.,-12.71524));
#17934=CARTESIAN_POINT('Origin',(0.,0.,-12.71524));
#17935=CARTESIAN_POINT('',(6.0325,-7.38768181585641E-16,-13.09624));
#17936=CARTESIAN_POINT('',(5.6515,-6.92109138538127E-16,-12.71524));
#17937=CARTESIAN_POINT('Origin',(0.,0.,-13.09624));
#17938=CARTESIAN_POINT('Origin',(0.,0.,-13.09624));
#17939=CARTESIAN_POINT('',(7.6835,-9.40957368124869E-16,-13.09624));
#17940=CARTESIAN_POINT('Origin',(0.,0.,-13.09624));
#17941=CARTESIAN_POINT('',(7.6835,-9.40957368124869E-16,13.09624));
#17942=CARTESIAN_POINT('',(7.6835,-9.40957368124869E-16,-13.09624));
#17943=CARTESIAN_POINT('Origin',(0.,0.,13.09624));
#17944=CARTESIAN_POINT('Origin',(0.,6.0325,-13.09624));
#17945=CARTESIAN_POINT('Origin',(0.,7.6835,13.09624));
#17946=CARTESIAN_POINT('',(0.,-7.4676,0.));
#17947=CARTESIAN_POINT('',(35.56,-69.85,20.32));
#17948=CARTESIAN_POINT('',(0.,-19.5072,0.));
#17949=CARTESIAN_POINT('',(35.56,-69.85,-21.2852000000001));
#17950=CARTESIAN_POINT('',(0.,38.1,0.));
#17951=CARTESIAN_POINT('',(0.,-9.8298,0.));
#17952=CARTESIAN_POINT('',(35.56,-69.85,-5.55111512312578E-14));
#17953=CARTESIAN_POINT('',(35.56,-69.85,-5.55111512312578E-14));
#17954=CARTESIAN_POINT('',(35.56,-69.85,-5.55111512312578E-14));
#17955=CARTESIAN_POINT('',(35.56,-69.85,-0.000635000000026587));
#17956=CARTESIAN_POINT('',(0.,0.,0.));
#17957=CARTESIAN_POINT('',(-225.732069029162,-25.8139305521406,-117.475));
#17958=CARTESIAN_POINT('',(-225.732069029142,-25.8139305521406,628.525000000007));
#17959=CARTESIAN_POINT('',(377.577930970838,-25.8139305521406,628.525));
#17960=CARTESIAN_POINT('',(-143.732069029162,-25.8139305521406,628.525));
#17961=CARTESIAN_POINT('',(167.722930970838,-30.5764305521406,115.525));
#17962=CARTESIAN_POINT('',(66.122930970838,-95.8139305521406,-156.65030169119));
#17963=CARTESIAN_POINT('',(420.077930970838,-28.8139305521406,596.524999999986));
#17964=CARTESIAN_POINT('',(-186.232069029162,-28.8139305521406,596.524999999986));
#17965=CARTESIAN_POINT('',(420.077930970838,-28.8139305521406,-85.4749999999855));
#17966=CARTESIAN_POINT('',(-186.232069029162,-28.8139305521406,-85.4749999999856));
#17967=UNCERTAINTY_MEASURE_WITH_UNIT(LENGTH_MEASURE(0.01),#18007,
'DISTANCE_ACCURACY_VALUE',
'Maximum model space distance between geometric entities at asserted c
onnectivities');
#17968=UNCERTAINTY_MEASURE_WITH_UNIT(LENGTH_MEASURE(0.01),#18007,
'DISTANCE_ACCURACY_VALUE',
'Maximum model space distance between geometric entities at asserted c
onnectivities');
#17969=UNCERTAINTY_MEASURE_WITH_UNIT(LENGTH_MEASURE(0.01),#18007,
'DISTANCE_ACCURACY_VALUE',
'Maximum model space distance between geometric entities at asserted c
onnectivities');
#17970=UNCERTAINTY_MEASURE_WITH_UNIT(LENGTH_MEASURE(0.01),#18007,
'DISTANCE_ACCURACY_VALUE',
'Maximum model space distance between geometric entities at asserted c
onnectivities');
#17971=UNCERTAINTY_MEASURE_WITH_UNIT(LENGTH_MEASURE(0.01),#18007,
'DISTANCE_ACCURACY_VALUE',
'Maximum model space distance between geometric entities at asserted c
onnectivities');
#17972=UNCERTAINTY_MEASURE_WITH_UNIT(LENGTH_MEASURE(0.01),#18007,
'DISTANCE_ACCURACY_VALUE',
'Maximum model space distance between geometric entities at asserted c
onnectivities');
#17973=UNCERTAINTY_MEASURE_WITH_UNIT(LENGTH_MEASURE(0.01),#18007,
'DISTANCE_ACCURACY_VALUE',
'Maximum model space distance between geometric entities at asserted c
onnectivities');
#17974=UNCERTAINTY_MEASURE_WITH_UNIT(LENGTH_MEASURE(0.01),#18007,
'DISTANCE_ACCURACY_VALUE',
'Maximum model space distance between geometric entities at asserted c
onnectivities');
#17975=UNCERTAINTY_MEASURE_WITH_UNIT(LENGTH_MEASURE(0.01),#18007,
'DISTANCE_ACCURACY_VALUE',
'Maximum model space distance between geometric entities at asserted c
onnectivities');
#17976=UNCERTAINTY_MEASURE_WITH_UNIT(LENGTH_MEASURE(0.01),#18007,
'DISTANCE_ACCURACY_VALUE',
'Maximum model space distance between geometric entities at asserted c
onnectivities');
#17977=UNCERTAINTY_MEASURE_WITH_UNIT(LENGTH_MEASURE(0.01),#18007,
'DISTANCE_ACCURACY_VALUE',
'Maximum model space distance between geometric entities at asserted c
onnectivities');
#17978=UNCERTAINTY_MEASURE_WITH_UNIT(LENGTH_MEASURE(0.01),#18007,
'DISTANCE_ACCURACY_VALUE',
'Maximum model space distance between geometric entities at asserted c
onnectivities');
#17979=UNCERTAINTY_MEASURE_WITH_UNIT(LENGTH_MEASURE(0.01),#18007,
'DISTANCE_ACCURACY_VALUE',
'Maximum model space distance between geometric entities at asserted c
onnectivities');
#17980=UNCERTAINTY_MEASURE_WITH_UNIT(LENGTH_MEASURE(0.01),#18007,
'DISTANCE_ACCURACY_VALUE',
'Maximum model space distance between geometric entities at asserted c
onnectivities');
#17981=UNCERTAINTY_MEASURE_WITH_UNIT(LENGTH_MEASURE(0.01),#18007,
'DISTANCE_ACCURACY_VALUE',
'Maximum model space distance between geometric entities at asserted c
onnectivities');
#17982=UNCERTAINTY_MEASURE_WITH_UNIT(LENGTH_MEASURE(0.01),#18007,
'DISTANCE_ACCURACY_VALUE',
'Maximum model space distance between geometric entities at asserted c
onnectivities');
#17983=UNCERTAINTY_MEASURE_WITH_UNIT(LENGTH_MEASURE(0.01),#18007,
'DISTANCE_ACCURACY_VALUE',
'Maximum model space distance between geometric entities at asserted c
onnectivities');
#17984=UNCERTAINTY_MEASURE_WITH_UNIT(LENGTH_MEASURE(0.01),#18007,
'DISTANCE_ACCURACY_VALUE',
'Maximum model space distance between geometric entities at asserted c
onnectivities');
#17985=UNCERTAINTY_MEASURE_WITH_UNIT(LENGTH_MEASURE(0.01),#18007,
'DISTANCE_ACCURACY_VALUE',
'Maximum model space distance between geometric entities at asserted c
onnectivities');
#17986=UNCERTAINTY_MEASURE_WITH_UNIT(LENGTH_MEASURE(0.01),#18007,
'DISTANCE_ACCURACY_VALUE',
'Maximum model space distance between geometric entities at asserted c
onnectivities');
#17987=(
GEOMETRIC_REPRESENTATION_CONTEXT(3)
GLOBAL_UNCERTAINTY_ASSIGNED_CONTEXT((#17967))
GLOBAL_UNIT_ASSIGNED_CONTEXT((#18007,#18009,#18010))
REPRESENTATION_CONTEXT('','3D')
);
#17988=(
GEOMETRIC_REPRESENTATION_CONTEXT(3)
GLOBAL_UNCERTAINTY_ASSIGNED_CONTEXT((#17968))
GLOBAL_UNIT_ASSIGNED_CONTEXT((#18007,#18009,#18010))
REPRESENTATION_CONTEXT('','3D')
);
#17989=(
GEOMETRIC_REPRESENTATION_CONTEXT(3)
GLOBAL_UNCERTAINTY_ASSIGNED_CONTEXT((#17969))
GLOBAL_UNIT_ASSIGNED_CONTEXT((#18007,#18009,#18010))
REPRESENTATION_CONTEXT('','3D')
);
#17990=(
GEOMETRIC_REPRESENTATION_CONTEXT(3)
GLOBAL_UNCERTAINTY_ASSIGNED_CONTEXT((#17970))
GLOBAL_UNIT_ASSIGNED_CONTEXT((#18007,#18009,#18010))
REPRESENTATION_CONTEXT('','3D')
);
#17991=(
GEOMETRIC_REPRESENTATION_CONTEXT(3)
GLOBAL_UNCERTAINTY_ASSIGNED_CONTEXT((#17971))
GLOBAL_UNIT_ASSIGNED_CONTEXT((#18007,#18009,#18010))
REPRESENTATION_CONTEXT('','3D')
);
#17992=(
GEOMETRIC_REPRESENTATION_CONTEXT(3)
GLOBAL_UNCERTAINTY_ASSIGNED_CONTEXT((#17972))
GLOBAL_UNIT_ASSIGNED_CONTEXT((#18007,#18009,#18010))
REPRESENTATION_CONTEXT('','3D')
);
#17993=(
GEOMETRIC_REPRESENTATION_CONTEXT(3)
GLOBAL_UNCERTAINTY_ASSIGNED_CONTEXT((#17973))
GLOBAL_UNIT_ASSIGNED_CONTEXT((#18007,#18009,#18010))
REPRESENTATION_CONTEXT('','3D')
);
#17994=(
GEOMETRIC_REPRESENTATION_CONTEXT(3)
GLOBAL_UNCERTAINTY_ASSIGNED_CONTEXT((#17974))
GLOBAL_UNIT_ASSIGNED_CONTEXT((#18007,#18009,#18010))
REPRESENTATION_CONTEXT('','3D')
);
#17995=(
GEOMETRIC_REPRESENTATION_CONTEXT(3)
GLOBAL_UNCERTAINTY_ASSIGNED_CONTEXT((#17975))
GLOBAL_UNIT_ASSIGNED_CONTEXT((#18007,#18009,#18010))
REPRESENTATION_CONTEXT('','3D')
);
#17996=(
GEOMETRIC_REPRESENTATION_CONTEXT(3)
GLOBAL_UNCERTAINTY_ASSIGNED_CONTEXT((#17976))
GLOBAL_UNIT_ASSIGNED_CONTEXT((#18007,#18009,#18010))
REPRESENTATION_CONTEXT('','3D')
);
#17997=(
GEOMETRIC_REPRESENTATION_CONTEXT(3)
GLOBAL_UNCERTAINTY_ASSIGNED_CONTEXT((#17977))
GLOBAL_UNIT_ASSIGNED_CONTEXT((#18007,#18009,#18010))
REPRESENTATION_CONTEXT('','3D')
);
#17998=(
GEOMETRIC_REPRESENTATION_CONTEXT(3)
GLOBAL_UNCERTAINTY_ASSIGNED_CONTEXT((#17978))
GLOBAL_UNIT_ASSIGNED_CONTEXT((#18007,#18009,#18010))
REPRESENTATION_CONTEXT('','3D')
);
#17999=(
GEOMETRIC_REPRESENTATION_CONTEXT(3)
GLOBAL_UNCERTAINTY_ASSIGNED_CONTEXT((#17979))
GLOBAL_UNIT_ASSIGNED_CONTEXT((#18007,#18009,#18010))
REPRESENTATION_CONTEXT('','3D')
);
#18000=(
GEOMETRIC_REPRESENTATION_CONTEXT(3)
GLOBAL_UNCERTAINTY_ASSIGNED_CONTEXT((#17980))
GLOBAL_UNIT_ASSIGNED_CONTEXT((#18007,#18009,#18010))
REPRESENTATION_CONTEXT('','3D')
);
#18001=(
GEOMETRIC_REPRESENTATION_CONTEXT(3)
GLOBAL_UNCERTAINTY_ASSIGNED_CONTEXT((#17981))
GLOBAL_UNIT_ASSIGNED_CONTEXT((#18007,#18009,#18010))
REPRESENTATION_CONTEXT('','3D')
);
#18002=(
GEOMETRIC_REPRESENTATION_CONTEXT(3)
GLOBAL_UNCERTAINTY_ASSIGNED_CONTEXT((#17982))
GLOBAL_UNIT_ASSIGNED_CONTEXT((#18007,#18009,#18010))
REPRESENTATION_CONTEXT('','3D')
);
#18003=(
GEOMETRIC_REPRESENTATION_CONTEXT(3)
GLOBAL_UNCERTAINTY_ASSIGNED_CONTEXT((#17983))
GLOBAL_UNIT_ASSIGNED_CONTEXT((#18007,#18009,#18010))
REPRESENTATION_CONTEXT('','3D')
);
#18004=(
GEOMETRIC_REPRESENTATION_CONTEXT(3)
GLOBAL_UNCERTAINTY_ASSIGNED_CONTEXT((#17984))
GLOBAL_UNIT_ASSIGNED_CONTEXT((#18007,#18009,#18010))
REPRESENTATION_CONTEXT('','3D')
);
#18005=(
GEOMETRIC_REPRESENTATION_CONTEXT(3)
GLOBAL_UNCERTAINTY_ASSIGNED_CONTEXT((#17985))
GLOBAL_UNIT_ASSIGNED_CONTEXT((#18007,#18009,#18010))
REPRESENTATION_CONTEXT('','3D')
);
#18006=(
GEOMETRIC_REPRESENTATION_CONTEXT(3)
GLOBAL_UNCERTAINTY_ASSIGNED_CONTEXT((#17986))
GLOBAL_UNIT_ASSIGNED_CONTEXT((#18007,#18009,#18010))
REPRESENTATION_CONTEXT('','3D')
);
#18007=(
LENGTH_UNIT()
NAMED_UNIT(*)
SI_UNIT(.MILLI.,.METRE.)
);
#18008=(
LENGTH_UNIT()
NAMED_UNIT(*)
SI_UNIT($,.METRE.)
);
#18009=(
NAMED_UNIT(*)
PLANE_ANGLE_UNIT()
SI_UNIT($,.RADIAN.)
);
#18010=(
NAMED_UNIT(*)
SI_UNIT($,.STERADIAN.)
SOLID_ANGLE_UNIT()
);
#18011=SHAPE_DEFINITION_REPRESENTATION(#18030,#18070);
#18012=SHAPE_DEFINITION_REPRESENTATION(#18031,#18071);
#18013=SHAPE_DEFINITION_REPRESENTATION(#18032,#18072);
#18014=SHAPE_DEFINITION_REPRESENTATION(#18033,#18073);
#18015=SHAPE_DEFINITION_REPRESENTATION(#18034,#18074);
#18016=SHAPE_DEFINITION_REPRESENTATION(#18035,#18075);
#18017=SHAPE_DEFINITION_REPRESENTATION(#18036,#18076);
#18018=SHAPE_DEFINITION_REPRESENTATION(#18037,#18077);
#18019=SHAPE_DEFINITION_REPRESENTATION(#18038,#18078);
#18020=SHAPE_DEFINITION_REPRESENTATION(#18039,#18079);
#18021=SHAPE_DEFINITION_REPRESENTATION(#18040,#18080);
#18022=SHAPE_DEFINITION_REPRESENTATION(#18041,#18081);
#18023=SHAPE_DEFINITION_REPRESENTATION(#18042,#18082);
#18024=SHAPE_DEFINITION_REPRESENTATION(#18043,#18083);
#18025=SHAPE_DEFINITION_REPRESENTATION(#18044,#18084);
#18026=SHAPE_DEFINITION_REPRESENTATION(#18045,#18085);
#18027=SHAPE_DEFINITION_REPRESENTATION(#18046,#18086);
#18028=SHAPE_DEFINITION_REPRESENTATION(#18047,#18087);
#18029=SHAPE_DEFINITION_REPRESENTATION(#18048,#18088);
#18030=PRODUCT_DEFINITION_SHAPE('',$,#18090);
#18031=PRODUCT_DEFINITION_SHAPE('',$,#18091);
#18032=PRODUCT_DEFINITION_SHAPE('',$,#18092);
#18033=PRODUCT_DEFINITION_SHAPE('',$,#18093);
#18034=PRODUCT_DEFINITION_SHAPE('',$,#18094);
#18035=PRODUCT_DEFINITION_SHAPE('',$,#18095);
#18036=PRODUCT_DEFINITION_SHAPE('',$,#18096);
#18037=PRODUCT_DEFINITION_SHAPE('',$,#18097);
#18038=PRODUCT_DEFINITION_SHAPE('',$,#18098);
#18039=PRODUCT_DEFINITION_SHAPE('',$,#18099);
#18040=PRODUCT_DEFINITION_SHAPE('',$,#18100);
#18041=PRODUCT_DEFINITION_SHAPE('',$,#18101);
#18042=PRODUCT_DEFINITION_SHAPE('',$,#18102);
#18043=PRODUCT_DEFINITION_SHAPE('',$,#18103);
#18044=PRODUCT_DEFINITION_SHAPE('',$,#18104);
#18045=PRODUCT_DEFINITION_SHAPE('',$,#18105);
#18046=PRODUCT_DEFINITION_SHAPE('',$,#18106);
#18047=PRODUCT_DEFINITION_SHAPE('',$,#18107);
#18048=PRODUCT_DEFINITION_SHAPE('',$,#18108);
#18049=PRODUCT_DEFINITION_SHAPE($,$,#74);
#18050=PRODUCT_DEFINITION_SHAPE($,$,#75);
#18051=PRODUCT_DEFINITION_SHAPE($,$,#76);
#18052=PRODUCT_DEFINITION_SHAPE($,$,#77);
#18053=PRODUCT_DEFINITION_SHAPE($,$,#78);
#18054=PRODUCT_DEFINITION_SHAPE($,$,#79);
#18055=PRODUCT_DEFINITION_SHAPE($,$,#80);
#18056=PRODUCT_DEFINITION_SHAPE($,$,#81);
#18057=PRODUCT_DEFINITION_SHAPE($,$,#82);
#18058=PRODUCT_DEFINITION_SHAPE($,$,#83);
#18059=PRODUCT_DEFINITION_SHAPE($,$,#84);
#18060=PRODUCT_DEFINITION_SHAPE($,$,#85);
#18061=PRODUCT_DEFINITION_SHAPE($,$,#86);
#18062=PRODUCT_DEFINITION_SHAPE($,$,#87);
#18063=PRODUCT_DEFINITION_SHAPE($,$,#88);
#18064=PRODUCT_DEFINITION_SHAPE($,$,#89);
#18065=PRODUCT_DEFINITION_SHAPE($,$,#90);
#18066=PRODUCT_DEFINITION_SHAPE($,$,#91);
#18067=PRODUCT_DEFINITION_SHAPE($,$,#92);
#18068=PRODUCT_DEFINITION_SHAPE($,$,#93);
#18069=PRODUCT_DEFINITION_SHAPE($,$,#94);
#18070=SHAPE_REPRESENTATION('',(#9749,#10851,#10852,#10853,#10854,#10855,
#10856,#10857,#10858,#10859,#10860),#17987);
#18071=SHAPE_REPRESENTATION('',(#9750),#17988);
#18072=SHAPE_REPRESENTATION('',(#9886),#17989);
#18073=SHAPE_REPRESENTATION('',(#10013),#17990);
#18074=SHAPE_REPRESENTATION('',(#10080),#17991);
#18075=SHAPE_REPRESENTATION('',(#10147),#17992);
#18076=SHAPE_REPRESENTATION('',(#10211),#17993);
#18077=SHAPE_REPRESENTATION('',(#10242,#10850),#17994);
#18078=SHAPE_REPRESENTATION('',(#10243,#10840,#10841,#10842,#10843,#10844,
#10845,#10846,#10847,#10848,#10849),#17995);
#18079=SHAPE_REPRESENTATION('',(#10244),#17996);
#18080=SHAPE_REPRESENTATION('',(#10508),#17997);
#18081=SHAPE_REPRESENTATION('',(#10546),#17998);
#18082=SHAPE_REPRESENTATION('',(#10592),#17999);
#18083=SHAPE_REPRESENTATION('',(#10635),#18000);
#18084=SHAPE_REPRESENTATION('',(#10683),#18001);
#18085=SHAPE_REPRESENTATION('',(#10733),#18002);
#18086=SHAPE_REPRESENTATION('',(#10772),#18003);
#18087=SHAPE_REPRESENTATION('',(#10817),#18004);
#18088=SHAPE_REPRESENTATION('',(#10826),#18005);
#18089=PRODUCT_DEFINITION_CONTEXT('part definition',#18148,'design');
#18090=PRODUCT_DEFINITION('MAT-018','MAT-018',#18109,#18089);
#18091=PRODUCT_DEFINITION('Bottom Rail','Bottom Rail',#18110,#18089);
#18092=PRODUCT_DEFINITION('Top Rail','Top Rail',#18111,#18089);
#18093=PRODUCT_DEFINITION('Right Upright','Right Upright',#18112,#18089);
#18094=PRODUCT_DEFINITION('Left Upright','Left Upright',#18113,#18089);
#18095=PRODUCT_DEFINITION('Mounting Strap','Mounting Strap',#18114,#18089);
#18096=PRODUCT_DEFINITION('Catch Tray','Catch Tray',#18115,#18089);
#18097=PRODUCT_DEFINITION('Swivel Caster Assembly',
'Swivel Caster Assembly',#18116,#18089);
#18098=PRODUCT_DEFINITION('Swivel Caster','Swivel Caster',#18117,#18089);
#18099=PRODUCT_DEFINITION('Caster Fork','Caster Fork',#18118,#18089);
#18100=PRODUCT_DEFINITION('Axle Bolt','Axle Bolt',#18119,#18089);
#18101=PRODUCT_DEFINITION('Swivel Bearing Plate','Swivel Bearing Plate',
#18120,#18089);
#18102=PRODUCT_DEFINITION('Axle Nut','Axle Nut',#18121,#18089);
#18103=PRODUCT_DEFINITION('Swivel Stem','Swivel Stem',#18122,#18089);
#18104=PRODUCT_DEFINITION('Caster Mounting Plate',
'Caster Mounting Plate',#18123,#18089);
#18105=PRODUCT_DEFINITION('Wheel Hub','Wheel Hub',#18124,#18089);
#18106=PRODUCT_DEFINITION('Wheel Tire','Wheel Tire',#18125,#18089);
#18107=PRODUCT_DEFINITION('Axle Spacer','Axle Spacer',#18126,#18089);
#18108=PRODUCT_DEFINITION('Axle Bushing','Axle Bushing',#18127,#18089);
#18109=PRODUCT_DEFINITION_FORMATION('',$,#18150);
#18110=PRODUCT_DEFINITION_FORMATION('',$,#18151);
#18111=PRODUCT_DEFINITION_FORMATION('',$,#18152);
#18112=PRODUCT_DEFINITION_FORMATION('',$,#18153);
#18113=PRODUCT_DEFINITION_FORMATION('',$,#18154);
#18114=PRODUCT_DEFINITION_FORMATION('',$,#18155);
#18115=PRODUCT_DEFINITION_FORMATION('',$,#18156);
#18116=PRODUCT_DEFINITION_FORMATION('',$,#18157);
#18117=PRODUCT_DEFINITION_FORMATION('',$,#18158);
#18118=PRODUCT_DEFINITION_FORMATION('',$,#18159);
#18119=PRODUCT_DEFINITION_FORMATION('',$,#18160);
#18120=PRODUCT_DEFINITION_FORMATION('',$,#18161);
#18121=PRODUCT_DEFINITION_FORMATION('',$,#18162);
#18122=PRODUCT_DEFINITION_FORMATION('',$,#18163);
#18123=PRODUCT_DEFINITION_FORMATION('',$,#18164);
#18124=PRODUCT_DEFINITION_FORMATION('',$,#18165);
#18125=PRODUCT_DEFINITION_FORMATION('',$,#18166);
#18126=PRODUCT_DEFINITION_FORMATION('',$,#18167);
#18127=PRODUCT_DEFINITION_FORMATION('',$,#18168);
#18128=PRODUCT_RELATED_PRODUCT_CATEGORY('MAT-018','MAT-018',(#18150));
#18129=PRODUCT_RELATED_PRODUCT_CATEGORY('Bottom Rail','Bottom Rail',(#18151));
#18130=PRODUCT_RELATED_PRODUCT_CATEGORY('Top Rail','Top Rail',(#18152));
#18131=PRODUCT_RELATED_PRODUCT_CATEGORY('Right Upright','Right Upright',
(#18153));
#18132=PRODUCT_RELATED_PRODUCT_CATEGORY('Left Upright','Left Upright',(#18154));
#18133=PRODUCT_RELATED_PRODUCT_CATEGORY('Mounting Strap',
'Mounting Strap',(#18155));
#18134=PRODUCT_RELATED_PRODUCT_CATEGORY('Catch Tray','Catch Tray',(#18156));
#18135=PRODUCT_RELATED_PRODUCT_CATEGORY('Swivel Caster Assembly',
'Swivel Caster Assembly',(#18157));
#18136=PRODUCT_RELATED_PRODUCT_CATEGORY('Swivel Caster','Swivel Caster',
(#18158));
#18137=PRODUCT_RELATED_PRODUCT_CATEGORY('Caster Fork','Caster Fork',(#18159));
#18138=PRODUCT_RELATED_PRODUCT_CATEGORY('Axle Bolt','Axle Bolt',(#18160));
#18139=PRODUCT_RELATED_PRODUCT_CATEGORY('Swivel Bearing Plate',
'Swivel Bearing Plate',(#18161));
#18140=PRODUCT_RELATED_PRODUCT_CATEGORY('Axle Nut','Axle Nut',(#18162));
#18141=PRODUCT_RELATED_PRODUCT_CATEGORY('Swivel Stem','Swivel Stem',(#18163));
#18142=PRODUCT_RELATED_PRODUCT_CATEGORY('Caster Mounting Plate',
'Caster Mounting Plate',(#18164));
#18143=PRODUCT_RELATED_PRODUCT_CATEGORY('Wheel Hub','Wheel Hub',(#18165));
#18144=PRODUCT_RELATED_PRODUCT_CATEGORY('Wheel Tire','Wheel Tire',(#18166));
#18145=PRODUCT_RELATED_PRODUCT_CATEGORY('Axle Spacer','Axle Spacer',(#18167));
#18146=PRODUCT_RELATED_PRODUCT_CATEGORY('Axle Bushing','Axle Bushing',(#18168));
#18147=APPLICATION_PROTOCOL_DEFINITION('international standard',
'automotive_design',2009,#18148);
#18148=APPLICATION_CONTEXT(
'Core Data for Automotive Mechanical Design Process');
#18149=PRODUCT_CONTEXT('part definition',#18148,'mechanical');
#18150=PRODUCT('MAT-018','MAT-018','STEP AP214',(#18149));
#18151=PRODUCT('Bottom Rail','Bottom Rail',$,(#18149));
#18152=PRODUCT('Top Rail','Top Rail',$,(#18149));
#18153=PRODUCT('Right Upright','Right Upright',$,(#18149));
#18154=PRODUCT('Left Upright','Left Upright',$,(#18149));
#18155=PRODUCT('Mounting Strap','Mounting Strap',$,(#18149));
#18156=PRODUCT('Catch Tray','Catch Tray',$,(#18149));
#18157=PRODUCT('Swivel Caster Assembly','Swivel Caster Assembly',$,(#18149));
#18158=PRODUCT('Swivel Caster','Swivel Caster',$,(#18149));
#18159=PRODUCT('Caster Fork','Caster Fork',$,(#18149));
#18160=PRODUCT('Axle Bolt','Axle Bolt',$,(#18149));
#18161=PRODUCT('Swivel Bearing Plate','Swivel Bearing Plate',$,(#18149));
#18162=PRODUCT('Axle Nut','Axle Nut',$,(#18149));
#18163=PRODUCT('Swivel Stem','Swivel Stem',$,(#18149));
#18164=PRODUCT('Caster Mounting Plate','Caster Mounting Plate',$,(#18149));
#18165=PRODUCT('Wheel Hub','Wheel Hub',$,(#18149));
#18166=PRODUCT('Wheel Tire','Wheel Tire',$,(#18149));
#18167=PRODUCT('Axle Spacer','Axle Spacer',$,(#18149));
#18168=PRODUCT('Axle Bushing','Axle Bushing',$,(#18149));
#18169=PRESENTATION_STYLE_ASSIGNMENT((#18173));
#18170=PRESENTATION_STYLE_ASSIGNMENT((#18174));
#18171=PRESENTATION_STYLE_ASSIGNMENT((#18175));
#18172=PRESENTATION_STYLE_ASSIGNMENT((#18176));
#18173=SURFACE_STYLE_USAGE(.BOTH.,#18177);
#18174=SURFACE_STYLE_USAGE(.BOTH.,#18178);
#18175=SURFACE_STYLE_USAGE(.BOTH.,#18179);
#18176=SURFACE_STYLE_USAGE(.BOTH.,#18180);
#18177=SURFACE_SIDE_STYLE('',(#18181));
#18178=SURFACE_SIDE_STYLE('',(#18182));
#18179=SURFACE_SIDE_STYLE('',(#18183));
#18180=SURFACE_SIDE_STYLE('',(#18184));
#18181=SURFACE_STYLE_FILL_AREA(#18185);
#18182=SURFACE_STYLE_FILL_AREA(#18186);
#18183=SURFACE_STYLE_FILL_AREA(#18187);
#18184=SURFACE_STYLE_FILL_AREA(#18188);
#18185=FILL_AREA_STYLE('Steel - Satin',(#18189));
#18186=FILL_AREA_STYLE('Opaque(227,224,212)',(#18190));
#18187=FILL_AREA_STYLE('Opaque(61,176,222)',(#18191));
#18188=FILL_AREA_STYLE('Opaque(97,158,199)',(#18192));
#18189=FILL_AREA_STYLE_COLOUR('Steel - Satin',#18193);
#18190=FILL_AREA_STYLE_COLOUR('Opaque(227,224,212)',#18194);
#18191=FILL_AREA_STYLE_COLOUR('Opaque(61,176,222)',#18195);
#18192=FILL_AREA_STYLE_COLOUR('Opaque(97,158,199)',#18196);
#18193=COLOUR_RGB('Steel - Satin',0.627450980392157,0.627450980392157,0.627450980392157);
#18194=COLOUR_RGB('Opaque(227,224,212)',0.890196078431372,0.87843137254902,
0.831372549019608);
#18195=COLOUR_RGB('Opaque(61,176,222)',0.23921568627451,0.690196078431373,
0.870588235294118);
#18196=COLOUR_RGB('Opaque(97,158,199)',0.380392156862745,0.619607843137255,
0.780392156862745);
ENDSEC;
END-ISO-10303-21;
